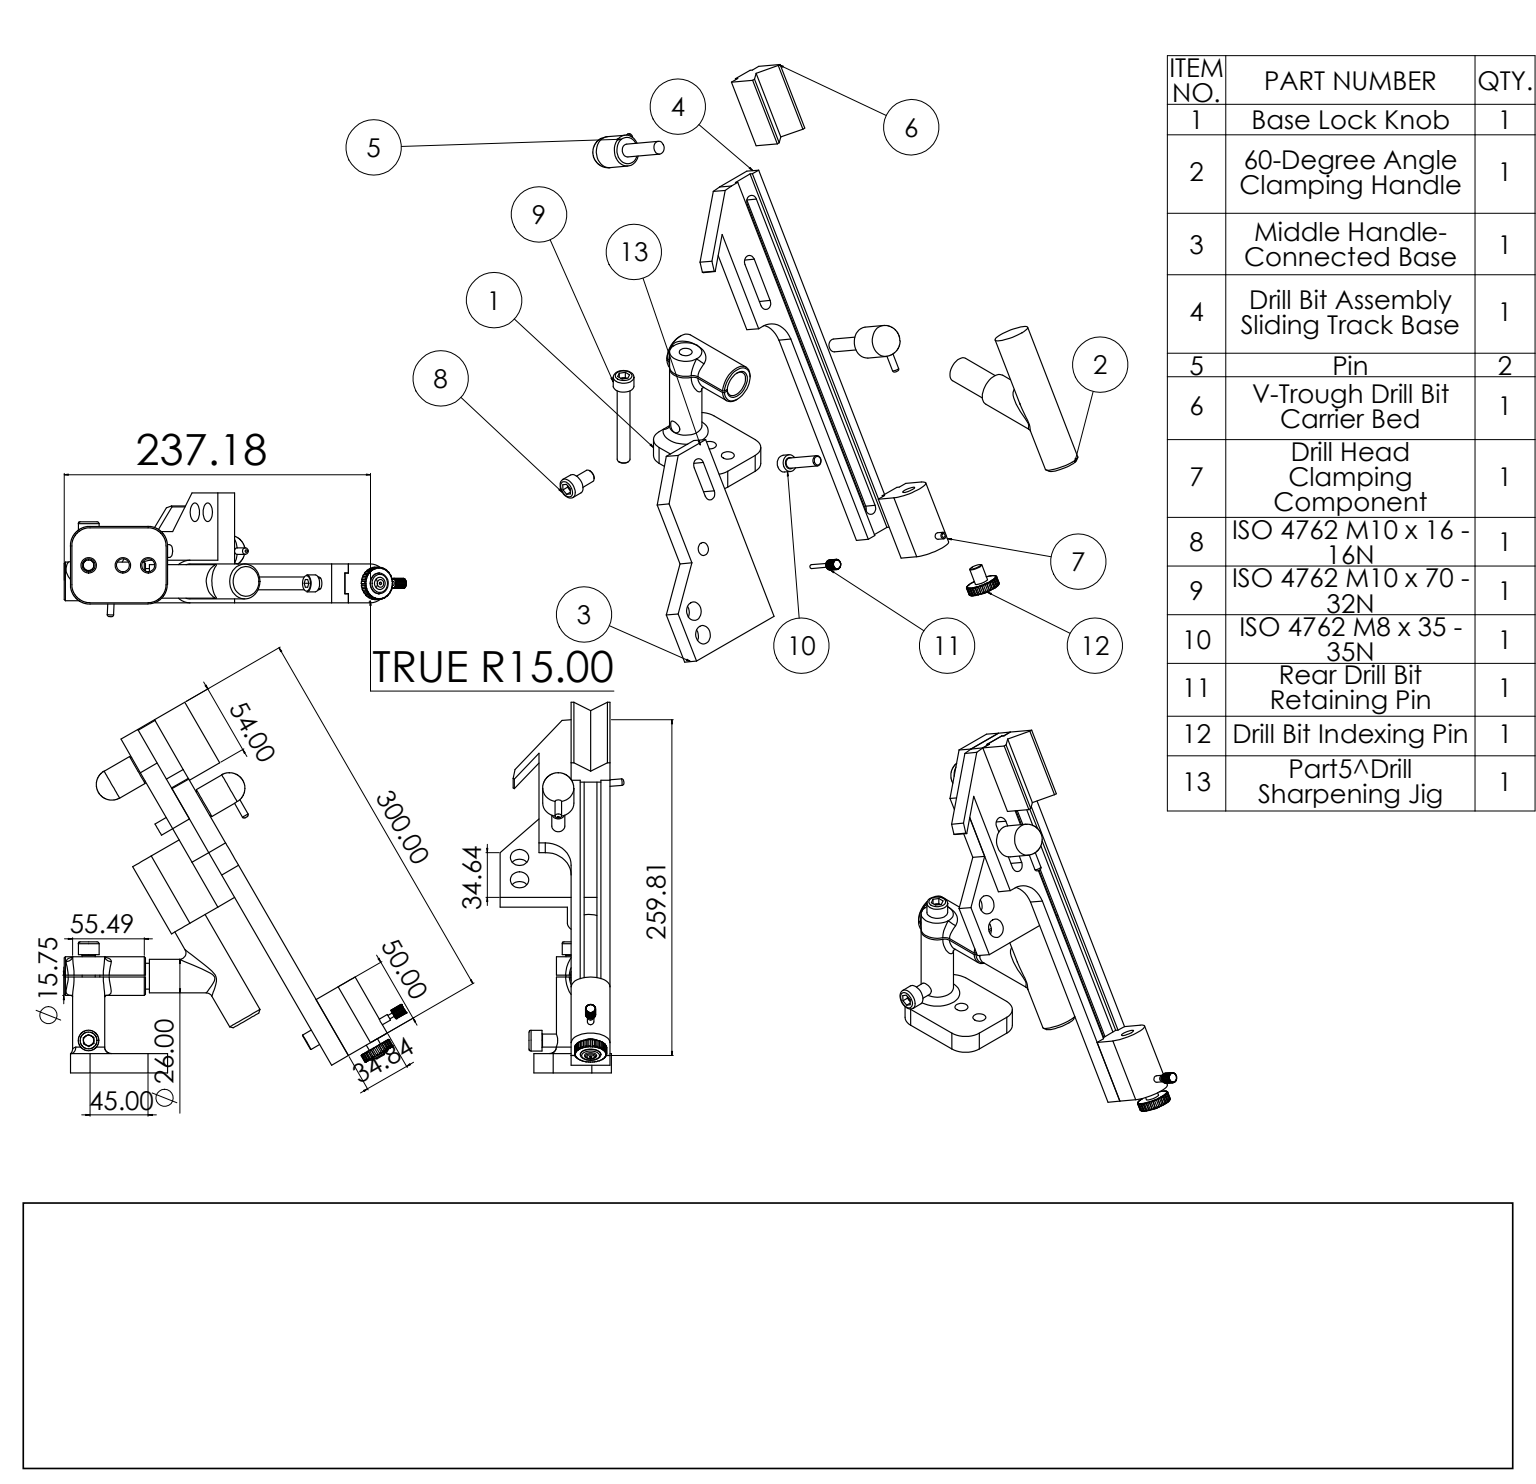
ISO-10303-21;
HEADER;
FILE_DESCRIPTION (('STEP AP214'),
    '1' );
FILE_NAME ('MAS-328',
    '2026-10-26T22:46:44',
    ( '' ),
    ( '' ),
    'SwSTEP 2.0',
    'SolidWorks 2025',
    '' );
FILE_SCHEMA (( 'AUTOMOTIVE_DESIGN' ));
ENDSEC;

DATA;
#1 = PLANE ( 'NONE',  #9182 ) ;
#2 = FACE_OUTER_BOUND ( 'NONE', #11522, .T. ) ;
#3 = CARTESIAN_POINT ( 'NONE',  ( 65.59213978856993776, 73.13321318536134186, -22.65145034150330616 ) ) ;
#4 = DIRECTION ( 'NONE',  ( 0.000000000000000000, 0.4999999999999984457, -0.8660254037844395958 ) ) ;
#5 = DIRECTION ( 'NONE',  ( -0.5000000000000047740, 0.8660254037844358210, 0.000000000000000000 ) ) ;
#6 = ORIENTED_EDGE ( 'NONE', *, *, #8024, .T. ) ;
#7 = CARTESIAN_POINT ( 'NONE',  ( 63.07699891084844523, 77.89006876494195808, -8.475025019650114899 ) ) ;
#8 = VECTOR ( 'NONE', #14091, 1000.000000000000227 ) ;
#9 = ORIENTED_EDGE ( 'NONE', *, *, #6510, .F. ) ;
#10 = ORIENTED_EDGE ( 'NONE', *, *, #14818, .T. ) ;
#11 = CARTESIAN_POINT ( 'NONE',  ( 221.3517569193846271, 32.83641968311255965, -11.78314368930809231 ) ) ;
#12 = CARTESIAN_POINT ( 'NONE',  ( 221.2462657448135417, 31.50562936879607889, -12.30768923015401128 ) ) ;
#13 = EDGE_CURVE ( 'NONE', #4124, #14697, #820, .T. ) ;
#14 = ORIENTED_EDGE ( 'NONE', *, *, #6610, .T. ) ;
#15 = CARTESIAN_POINT ( 'NONE',  ( -25.96080279087190945, 79.85293219504170281, -10.39653350028737755 ) ) ;
#16 = DIRECTION ( 'NONE',  ( -0.8660254037844355990, -0.5000000000000055511, 0.000000000000000000 ) ) ;
#17 = ORIENTED_EDGE ( 'NONE', *, *, #2123, .F. ) ;
#18 = AXIS2_PLACEMENT_3D ( 'NONE', #4792, #10950, #15638 ) ;
#19 = CARTESIAN_POINT ( 'NONE',  ( 0.000000000000000000, -10.00000000000000000, 0.000000000000000000 ) ) ;
#20 = LINE ( 'NONE', #125, #6600 ) ;
#21 = LINE ( 'NONE', #16230, #18993 ) ;
#22 = VECTOR ( 'NONE', #7023, 1000.000000000000114 ) ;
#23 = FACE_OUTER_BOUND ( 'NONE', #2829, .T. ) ;
#24 = CARTESIAN_POINT ( 'NONE',  ( 211.0853526979653907, 12.80985690719961312, -24.65893733905802776 ) ) ;
#25 = AXIS2_PLACEMENT_3D ( 'NONE', #18547, #841, #7289 ) ;
#26 = DIRECTION ( 'NONE',  ( 0.5000000000000044409, -0.8660254037844360431, -4.006172263299080068E-16 ) ) ;
#27 = EDGE_CURVE ( 'NONE', #5527, #10122, #12164, .T. ) ;
#28 = DIRECTION ( 'NONE',  ( -0.000000000000000000, 1.355657144061424088E-15, 1.000000000000000000 ) ) ;
#29 = CARTESIAN_POINT ( 'NONE',  ( 227.9553588074475670, 39.88513931160575510, -14.00000000000005507 ) ) ;
#30 = ORIENTED_EDGE ( 'NONE', *, *, #4834, .F. ) ;
#31 = DIRECTION ( 'NONE',  ( -0.2483788854153071712, -0.1434016163555487389, -0.9579895123154875680 ) ) ;
#32 = VECTOR ( 'NONE', #7463, 1000.000000000000114 ) ;
#33 = CARTESIAN_POINT ( 'NONE',  ( 72.20123527641440830, 74.90140838070377072, -0.9291223156572469000 ) ) ;
#34 = LINE ( 'NONE', #11272, #10471 ) ;
#35 = CARTESIAN_POINT ( 'NONE',  ( 214.5488276859554162, 7.740514238813806180, -25.36561010639692881 ) ) ;
#36 = EDGE_CURVE ( 'NONE', #14580, #7029, #1544, .T. ) ;
#38 = VERTEX_POINT ( 'NONE', #5675 ) ;
#37 = EDGE_LOOP ( 'NONE', ( #2124, #18268, #20120, #14576, #10012 ) ) ;
#39 = EDGE_CURVE ( 'NONE', #7899, #11760, #18628, .T. ) ;
#40 = CARTESIAN_POINT ( 'NONE',  ( -32.23733050826358237, 69.70612202061964524, 1.777571403100950187 ) ) ;
#41 = ORIENTED_EDGE ( 'NONE', *, *, #857, .F. ) ;
#42 = CYLINDRICAL_SURFACE ( 'NONE', #6692, 5.000000000000002665 ) ;
#43 = B_SPLINE_CURVE_WITH_KNOTS ( 'NONE', 3,
 ( #9463, #2715, #6285, #20719 ),
 .UNSPECIFIED., .F., .F.,
 ( 4, 4 ),
 ( 9.419794497943025677E-05, 0.0009481836829574997018 ),
 .UNSPECIFIED. ) ;
#44 = CARTESIAN_POINT ( 'NONE',  ( -28.41953442586123302, 80.00000000005270806, -1.424835221693572684 ) ) ;
#45 = CARTESIAN_POINT ( 'NONE',  ( 43.00000000000000000, 0.000000000000000000, 0.000000000000000000 ) ) ;
#46 = VECTOR ( 'NONE', #10219, 1000.000000000000227 ) ;
#47 = CIRCLE ( 'NONE', #14620, 8.000000000000058620 ) ;
#48 = CARTESIAN_POINT ( 'NONE',  ( 218.4949601902774248, 36.27103037639907512, -10.80501622924627902 ) ) ;
#49 = AXIS2_PLACEMENT_3D ( 'NONE', #5119, #19642, #8405 ) ;
#50 = CARTESIAN_POINT ( 'NONE',  ( 54.22345804136912051, 78.00945976696758066, -12.46744236580036791 ) ) ;
#51 = PRODUCT_RELATED_PRODUCT_CATEGORY ( 'part', '', ( #13821 ) ) ;
#52 = LINE ( 'NONE', #20812, #10386 ) ;
#53 = ORIENTED_EDGE ( 'NONE', *, *, #309, .F. ) ;
#54 =( LENGTH_UNIT ( ) NAMED_UNIT ( * ) SI_UNIT ( .MILLI., .METRE. ) );
#55 = PLANE ( 'NONE',  #11183 ) ;
#56 = ORIENTED_EDGE ( 'NONE', *, *, #8456, .T. ) ;
#57 = CARTESIAN_POINT ( 'NONE',  ( 80.00000000000000000, 0.000000000000000000, 0.000000000000000000 ) ) ;
#58 = ADVANCED_FACE ( 'NONE', ( #8662 ), #15261, .F. ) ;
#59 = AXIS2_PLACEMENT_3D ( 'NONE', #20205, #816, #18936 ) ;
#60 = ORIENTED_EDGE ( 'NONE', *, *, #4152, .T. ) ;
#61 = EDGE_CURVE ( 'NONE', #19064, #20850, #19152, .T. ) ;
#62 = LINE ( 'NONE', #1856, #5490 ) ;
#63 = CARTESIAN_POINT ( 'NONE',  ( 213.9541640218532166, 4.979392293579961937, -14.00000000000005507 ) ) ;
#64 = CARTESIAN_POINT ( 'NONE',  ( 220.2412569556373398, 35.17173234550051575, -17.78601433598970871 ) ) ;
#65 = CIRCLE ( 'NONE', #5111, 12.50000000000000000 ) ;
#66 = B_SPLINE_CURVE_WITH_KNOTS ( 'NONE', 3,
 ( #8841, #10417, #10308, #18497, #16902, #3750, #6925, #16700, #20081, #8735, #685, #15341, #16481, #1963, #8630, #5225, #15026, #3643, #15129, #584, #2382, #3544, #11613, #795, #7034, #9988, #7140, #8411, #10096, #5431, #7246, #2073, #5545, #13520, #19652, #19965, #12034, #14912, #20596, #12135, #15751, #14164, #15438, #7666 ),
 .UNSPECIFIED., .F., .F.,
 ( 4, 2, 2, 2, 2, 2, 2, 2, 2, 2, 2, 2, 2, 2, 2, 2, 2, 2, 2, 2, 2, 4 ),
 ( 0.09617483233575800650, 0.09914136407045009980, 0.1006246299377961534, 0.1021078958051422070, 0.1050744275398343142, 0.1080409592745264352, 0.1095242251418725027, 0.1110074910092185702, 0.1139740227439106635, 0.1154572886112567032, 0.1169405544786027568, 0.1176821874122757766, 0.1184238203459488104, 0.1199070862132948084, 0.1213903520806408065, 0.1228736179479868185, 0.1258401496826788146, 0.1288066814173708385, 0.1317732131520628625, 0.1377062766214468548, 0.1406728083561389064, 0.1436393400908309581 ),
 .UNSPECIFIED. ) ;
#67 = AXIS2_PLACEMENT_3D ( 'NONE', #10593, #11884, #4139 ) ;
#68 = CARTESIAN_POINT ( 'NONE',  ( 204.1847125716027733, 2.529609678273321727, -2.551678190571418092 ) ) ;
#69 = CARTESIAN_POINT ( 'NONE',  ( -27.55705705607979894, 6.378909713838078588, -4.810857297669037358 ) ) ;
#70 = CARTESIAN_POINT ( 'NONE',  ( 192.7136026671465174, 6.680946580180795458, -11.01983352639493141 ) ) ;
#71 = ORIENTED_EDGE ( 'NONE', *, *, #7515, .F. ) ;
#72 = ADVANCED_FACE ( 'NONE', ( #4104, #6856 ), #20110, .T. ) ;
#73 = DIRECTION ( 'NONE',  ( -1.000000000000000000, -0.000000000000000000, -0.000000000000000000 ) ) ;
#74 = CARTESIAN_POINT ( 'NONE',  ( -3.712242387446013758, 47.26449505096422854, -2.316332963494041497 ) ) ;
#75 = AXIS2_PLACEMENT_3D ( 'NONE', #8179, #20707, #4902 ) ;
#76 = ORIENTED_EDGE ( 'NONE', *, *, #3037, .F. ) ;
#77 = CARTESIAN_POINT ( 'NONE',  ( 199.2231352798573027, 21.03391272677540513, -14.00000000000005507 ) ) ;
#78 = CARTESIAN_POINT ( 'NONE',  ( -4.898149591010308335, 50.01850704181430984, -13.27720951148779349 ) ) ;
#79 = CARTESIAN_POINT ( 'NONE',  ( 25.17200000000003612, 0.000000000000000000, 0.000000000000000000 ) ) ;
#80 = VECTOR ( 'NONE', #13900, 1000.000000000000227 ) ;
#81 = AXIS2_PLACEMENT_3D ( 'NONE', #9573, #7982, #13089 ) ;
#82 = EDGE_CURVE ( 'NONE', #14650, #1521, #9980, .T. ) ;
#83 = CARTESIAN_POINT ( 'NONE',  ( 215.3534639294407782, 15.62807865697965504, -9.913166705713923221 ) ) ;
#84 = AXIS2_PLACEMENT_3D ( 'NONE', #10451, #8972, #10240 ) ;
#85 = CARTESIAN_POINT ( 'NONE',  ( 218.1772659767879361, 38.33479928385730062, -13.56204498775452372 ) ) ;
#87 = ORIENTED_EDGE ( 'NONE', *, *, #4132, .T. ) ;
#86 = ORIENTED_EDGE ( 'NONE', *, *, #18700, .F. ) ;
#88 = EDGE_LOOP ( 'NONE', ( #5156, #19517 ) ) ;
#89 = CARTESIAN_POINT ( 'NONE',  ( 204.5373383384513772, 2.217977392850209561, -25.12838443884007944 ) ) ;
#90 = FACE_OUTER_BOUND ( 'NONE', #11303, .T. ) ;
#91 = EDGE_CURVE ( 'NONE', #17637, #19670, #15056, .T. ) ;
#92 = ORIENTED_EDGE ( 'NONE', *, *, #17549, .F. ) ;
#93 = ORIENTED_EDGE ( 'NONE', *, *, #14481, .F. ) ;
#94 = CARTESIAN_POINT ( 'NONE',  ( -20.20766917169448007, 62.83385617594171180, -2.712160011935111914 ) ) ;
#95 = DIRECTION ( 'NONE',  ( -0.5000000000000042188, 0.8660254037844362651, -2.168404344971015524E-16 ) ) ;
#96 = DIRECTION ( 'NONE',  ( 0.7500000000000014433, 0.4330127018922259596, 0.4999999999999919509 ) ) ;
#97 = CARTESIAN_POINT ( 'NONE',  ( -14.59739189792666281, 58.60404727593866170, -4.812026853405405369 ) ) ;
#98 = EDGE_LOOP ( 'NONE', ( #990, #8694, #13068, #17263 ) ) ;
#99 = ORIENTED_EDGE ( 'NONE', *, *, #8969, .F. ) ;
#100 = FACE_OUTER_BOUND ( 'NONE', #9004, .T. ) ;
#101 = AXIS2_PLACEMENT_3D ( 'NONE', #17519, #19410, #6254 ) ;
#102 = ADVANCED_FACE ( 'NONE', ( #18525 ), #10234, .F. ) ;
#103 = CIRCLE ( 'NONE', #7142, 11.94520687646042667 ) ;
#104 = EDGE_CURVE ( 'NONE', #402, #10896, #9651, .T. ) ;
#105 = CARTESIAN_POINT ( 'NONE',  ( 218.1841183754832230, 38.29290577510303706, -13.37096421021187354 ) ) ;
#106 = CARTESIAN_POINT ( 'NONE',  ( 199.3420759002524960, 10.50789738563077513, -26.10173121575770239 ) ) ;
#107 = CARTESIAN_POINT ( 'NONE',  ( -32.72405129661866141, 57.94895811088655080, 0.7443064298479508123 ) ) ;
#108 = CARTESIAN_POINT ( 'NONE',  ( 209.9458835816058411, 16.63000860489531263, -23.47937149798938350 ) ) ;
#109 = ADVANCED_FACE ( 'NONE', ( #2310 ), #10446, .F. ) ;
#110 = FACE_OUTER_BOUND ( 'NONE', #8894, .T. ) ;
#111 = LINE ( 'NONE', #3275, #10000 ) ;
#112 = VERTEX_POINT ( 'NONE', #8556 ) ;
#113 = ORIENTED_EDGE ( 'NONE', *, *, #4613, .F. ) ;
#114 = CARTESIAN_POINT ( 'NONE',  ( 60.67510459333478678, 75.25732190833497270, -4.504626686252581891 ) ) ;
#115 = ORIENTED_EDGE ( 'NONE', *, *, #18818, .F. ) ;
#116 = DIRECTION ( 'NONE',  ( -0.8660254037844363761, -0.5000000000000043299, 6.872020471724002955E-17 ) ) ;
#117 = DIRECTION ( 'NONE',  ( -0.5000000000000029976, 0.8660254037844370423, 0.000000000000000000 ) ) ;
#118 = EDGE_CURVE ( 'NONE', #7633, #8779, #11849, .T. ) ;
#119 = ORIENTED_EDGE ( 'NONE', *, *, #8707, .T. ) ;
#120 = CARTESIAN_POINT ( 'NONE',  ( 184.9952905943350743, 3.535126980567765642, 0.9999999999999187317 ) ) ;
#121 = DIRECTION ( 'NONE',  ( -0.7071067811865331398, 8.659560562355110352E-17, -0.7071067811865620056 ) ) ;
#122 = VERTEX_POINT ( 'NONE', #2105 ) ;
#123 = APPLICATION_CONTEXT ( 'automotive_design' ) ;
#124 = CYLINDRICAL_SURFACE ( 'NONE', #4697, 7.155882939242642848 ) ;
#125 = CARTESIAN_POINT ( 'NONE',  ( 74.11964624731606932, 223.5773763115391262, -13.99999999999998757 ) ) ;
#126 = CARTESIAN_POINT ( 'NONE',  ( -0.1767699604045824824, 64.25000000000000000, 2.481238266578627449 ) ) ;
#127 = CARTESIAN_POINT ( 'NONE',  ( 221.7203120311961584, 32.40398170487073770, -15.50530648567724157 ) ) ;
#128 = DIRECTION ( 'NONE',  ( 0.5000000000000054401, -0.8660254037844354880, 0.000000000000000000 ) ) ;
#129 = DIRECTION ( 'NONE',  ( 0.000000000000000000, -0.5000000000000009992, -0.8660254037844380415 ) ) ;
#130 = CARTESIAN_POINT ( 'NONE',  ( 43.00000000000000000, 4.052968581778165278E-16, -3.309499999999999886 ) ) ;
#131 = ORIENTED_EDGE ( 'NONE', *, *, #17184, .F. ) ;
#132 = ORIENTED_EDGE ( 'NONE', *, *, #6398, .F. ) ;
#133 = DIRECTION ( 'NONE',  ( -0.000000000000000000, 1.000000000000000000, -0.000000000000000000 ) ) ;
#134 = CARTESIAN_POINT ( 'NONE',  ( 79.71489363099678371, 68.48589378271981332, 0.4850882486192328313 ) ) ;
#135 = CARTESIAN_POINT ( 'NONE',  ( 221.3208164193364951, 32.89001020120745267, -16.29291827778590118 ) ) ;
#136 = AXIS2_PLACEMENT_3D ( 'NONE', #13684, #12192, #17075 ) ;
#137 = CARTESIAN_POINT ( 'NONE',  ( 78.24291704612552678, 52.61578353862905288, -16.49051273642769289 ) ) ;
#138 = VECTOR ( 'NONE', #4761, 1000.000000000000114 ) ;
#140 = VERTEX_POINT ( 'NONE', #15368 ) ;
#139 = VERTEX_POINT ( 'NONE', #19892 ) ;
#141 = CARTESIAN_POINT ( 'NONE',  ( 226.3069872472380837, 42.74020260364054025, -12.62147488791602612 ) ) ;
#142 = VERTEX_POINT ( 'NONE', #18313 ) ;
#143 = CARTESIAN_POINT ( 'NONE',  ( -31.87136685185827645, 66.76123571212177410, 2.404802591979305237 ) ) ;
#144 = ORIENTED_EDGE ( 'NONE', *, *, #2804, .F. ) ;
#145 = CYLINDRICAL_SURFACE ( 'NONE', #15851, 12.47473710546057646 ) ;
#146 = DIRECTION ( 'NONE',  ( -1.000000000000000000, -0.000000000000000000, -0.000000000000000000 ) ) ;
#147 = CARTESIAN_POINT ( 'NONE',  ( 59.39721438298058587, 215.0773763115390125, -5.999999999999973355 ) ) ;
#148 = AXIS2_PLACEMENT_3D ( 'NONE', #15807, #6608, #5027 ) ;
#149 = CARTESIAN_POINT ( 'NONE',  ( 55.21771490548105987, 77.58705400462579860, -9.223793769219156502 ) ) ;
#150 = EDGE_CURVE ( 'NONE', #14752, #17095, #8765, .T. ) ;
#151 = CARTESIAN_POINT ( 'NONE',  ( -28.39898833977742854, 64.25000000000000000, 3.829121630900767848 ) ) ;
#152 = ORIENTED_EDGE ( 'NONE', *, *, #1114, .F. ) ;
#153 = DIRECTION ( 'NONE',  ( 0.8660254037844380415, 0.5000000000000014433, 0.000000000000000000 ) ) ;
#154 = CARTESIAN_POINT ( 'NONE',  ( 189.6713070174558311, 31.72030020615783030, -9.000000000000065725 ) ) ;
#155 = ORIENTED_EDGE ( 'NONE', *, *, #17412, .T. ) ;
#156 = CARTESIAN_POINT ( 'NONE',  ( 220.9239438240024356, 32.06390731203414646, -15.46846178913028425 ) ) ;
#157 = EDGE_LOOP ( 'NONE', ( #6682, #1571, #19730, #8704 ) ) ;
#158 = CARTESIAN_POINT ( 'NONE',  ( 217.8938201104045618, 37.31223553720490571, -11.78314368930801770 ) ) ;
#159 = DIRECTION ( 'NONE',  ( 0.5000000000000054401, -0.8660254037844353769, 3.330669073875469128E-16 ) ) ;
#160 = LINE ( 'NONE', #8201, #12763 ) ;
#161 = AXIS2_PLACEMENT_3D ( 'NONE', #9354, #1324, #10848 ) ;
#162 = EDGE_CURVE ( 'NONE', #4703, #13744, #13389, .T. ) ;
#163 = CARTESIAN_POINT ( 'NONE',  ( 204.3649803021097568, 2.376073449241438595, -2.709673684914560621 ) ) ;
#164 = CARTESIAN_POINT ( 'NONE',  ( 228.9348979434486466, 38.18852776005019223, -17.77545290933962008 ) ) ;
#165 = CARTESIAN_POINT ( 'NONE',  ( 226.5371121300225923, 42.34161461457158993, -11.75146085096529269 ) ) ;
#166 = VERTEX_POINT ( 'NONE', #7371 ) ;
#167 = CARTESIAN_POINT ( 'NONE',  ( 64.57205371728791476, 77.00255147951500589, -18.47244162738281048 ) ) ;
#168 = CARTESIAN_POINT ( 'NONE',  ( -15.61408887313298166, 45.63508326896292289, -12.50000000000000533 ) ) ;
#169 = EDGE_CURVE ( 'NONE', #12266, #578, #4413, .T. ) ;
#170 = ORIENTED_EDGE ( 'NONE', *, *, #16678, .F. ) ;
#171 = EDGE_CURVE ( 'NONE', #6173, #11821, #2564, .T. ) ;
#172 = LINE ( 'NONE', #6717, #1739 ) ;
#173 = CARTESIAN_POINT ( 'NONE',  ( 0.8637328751229490509, 57.32143202600091314, 0.4056442452730588677 ) ) ;
#174 = CARTESIAN_POINT ( 'NONE',  ( 0.2936549083987780584, 78.35468191082874512, -5.667085693055155637 ) ) ;
#175 = DIRECTION ( 'NONE',  ( 0.8660254037844373753, 0.5000000000000021094, -5.551115123125781716E-16 ) ) ;
#176 = DIRECTION ( 'NONE',  ( 1.000000000000000000, 0.000000000000000000, 0.000000000000000000 ) ) ;
#177 = VECTOR ( 'NONE', #19876, 1000.000000000000114 ) ;
#179 = EDGE_LOOP ( 'NONE', ( #14684, #11009, #8415, #3507 ) ) ;
#178 = ORIENTED_EDGE ( 'NONE', *, *, #4682, .F. ) ;
#180 = ORIENTED_EDGE ( 'NONE', *, *, #8626, .T. ) ;
#181 = EDGE_LOOP ( 'NONE', ( #14178, #14869, #3890, #5041 ) ) ;
#182 = CARTESIAN_POINT ( 'NONE',  ( 5.000000000000004441, -2.342598717236899830, 4.057500000000059615 ) ) ;
#183 = DIRECTION ( 'NONE',  ( 0.000000000000000000, 0.000000000000000000, -1.000000000000000000 ) ) ;
#184 = VERTEX_POINT ( 'NONE', #12380 ) ;
#185 = ORIENTED_EDGE ( 'NONE', *, *, #2629, .T. ) ;
#186 = EDGE_CURVE ( 'NONE', #5696, #10545, #15103, .T. ) ;
#187 = CARTESIAN_POINT ( 'NONE',  ( 31.00000000000000711, 65.00000000000000000, 0.4999999999999970024 ) ) ;
#188 = CARTESIAN_POINT ( 'NONE',  ( 61.55523633728010680, 134.3395726428436774, -12.50000000000000000 ) ) ;
#189 = DIRECTION ( 'NONE',  ( -0.8660254037844360431, -0.5000000000000044409, 5.976026924694052093E-17 ) ) ;
#190 = CARTESIAN_POINT ( 'NONE',  ( 5.000000000000000000, -4.685197434473809430, 6.071532165918824830E-15 ) ) ;
#191 = ORIENTED_EDGE ( 'NONE', *, *, #11432, .T. ) ;
#192 = ORIENTED_EDGE ( 'NONE', *, *, #8358, .F. ) ;
#193 = CARTESIAN_POINT ( 'NONE',  ( 227.1212915979693037, 40.35032020428622701, -17.81526153211078523 ) ) ;
#194 = VECTOR ( 'NONE', #13444, 1000.000000000000000 ) ;
#195 = EDGE_CURVE ( 'NONE', #20338, #18465, #2729, .T. ) ;
#196 = VECTOR ( 'NONE', #4579, 1000.000000000000000 ) ;
#197 = VECTOR ( 'NONE', #8588, 1000.000000000000227 ) ;
#198 = PLANE ( 'NONE',  #5711 ) ;
#199 = ADVANCED_FACE ( 'NONE', ( #15570 ), #12386, .T. ) ;
#200 = CARTESIAN_POINT ( 'NONE',  ( 228.4406543832519674, 38.06511682656112328, -17.45257705044836172 ) ) ;
#201 = CARTESIAN_POINT ( 'NONE',  ( -32.31535884961043337, 59.90787884595005863, 1.627344972937480483 ) ) ;
#202 = CARTESIAN_POINT ( 'NONE',  ( 206.2111997916997552, 10.34978999605213978, -2.036337243043280676 ) ) ;
#203 = ORIENTED_EDGE ( 'NONE', *, *, #13292, .F. ) ;
#204 = DIRECTION ( 'NONE',  ( 0.8660254037844361541, 0.5000000000000043299, -5.976026924694053325E-17 ) ) ;
#205 = CARTESIAN_POINT ( 'NONE',  ( 221.1274251996601663, 33.84282198876892522, -17.45257705044835816 ) ) ;
#206 = VERTEX_POINT ( 'NONE', #13865 ) ;
#207 = CARTESIAN_POINT ( 'NONE',  ( 54.88115708448756891, 77.73008567377026168, -9.852707893755395574 ) ) ;
#208 = EDGE_CURVE ( 'NONE', #2385, #6975, #20515, .T. ) ;
#209 = ORIENTED_EDGE ( 'NONE', *, *, #20399, .T. ) ;
#210 = EDGE_CURVE ( 'NONE', #4589, #15417, #7306, .T. ) ;
#211 = VECTOR ( 'NONE', #12529, 1000.000000000000114 ) ;
#212 = CARTESIAN_POINT ( 'NONE',  ( 206.9147384664715048, 10.75597823931694563, -16.91825718831810477 ) ) ;
#213 = CIRCLE ( 'NONE', #14445, 0.4000000000000001887 ) ;
#214 = ORIENTED_EDGE ( 'NONE', *, *, #1106, .F. ) ;
#215 = CARTESIAN_POINT ( 'NONE',  ( 220.3379489458267528, 34.59238660243320851, -17.48830818005197330 ) ) ;
#216 = ORIENTED_EDGE ( 'NONE', *, *, #15468, .T. ) ;
#217 = ITEM_DEFINED_TRANSFORMATION ( 'NONE', 'NONE', #8397,  #18233 ) ;
#218 = EDGE_CURVE ( 'NONE', #14678, #19163, #6091, .T. ) ;
#219 = CARTESIAN_POINT ( 'NONE',  ( 203.2433706042751282, 14.07066088650062241, -14.00000000000004974 ) ) ;
#220 = ORIENTED_EDGE ( 'NONE', *, *, #3519, .T. ) ;
#221 = CIRCLE ( 'NONE', #10696, 3.047499999999999876 ) ;
#222 = FACE_OUTER_BOUND ( 'NONE', #14547, .T. ) ;
#223 = CYLINDRICAL_SURFACE ( 'NONE', #8286, 5.000000000000000000 ) ;
#224 = CIRCLE ( 'NONE', #4614, 1.000000000000000888 ) ;
#225 = CARTESIAN_POINT ( 'NONE',  ( 58.57586221349340860, 85.49999999999941735, -12.75852093573072032 ) ) ;
#226 = CARTESIAN_POINT ( 'NONE',  ( 9.999999999999994671, 5.551115123125782702E-17, 8.000000000000058620 ) ) ;
#227 = ADVANCED_FACE ( 'NONE', ( #9070 ), #12693, .F. ) ;
#228 = EDGE_LOOP ( 'NONE', ( #1966, #14551, #9394, #914, #2067, #12471, #14821, #17580, #5403, #1919 ) ) ;
#229 = DIRECTION ( 'NONE',  ( -0.5000000000000046629, 0.8660254037844360431, -0.000000000000000000 ) ) ;
#230 = DIRECTION ( 'NONE',  ( -0.5000000000000049960, 0.8660254037844358210, -0.000000000000000000 ) ) ;
#231 = DIRECTION ( 'NONE',  ( 0.8660254037844360431, 0.5000000000000044409, -5.976026924694052093E-17 ) ) ;
#232 = ORIENTED_EDGE ( 'NONE', *, *, #19491, .T. ) ;
#233 = DIRECTION ( 'NONE',  ( -0.8660254037844354880, -0.5000000000000055511, 0.000000000000000000 ) ) ;
#234 = ADVANCED_FACE ( 'NONE', ( #2627 ), #13079, .T. ) ;
#235 = CARTESIAN_POINT ( 'NONE',  ( 82.91273300024698756, 62.96352848655696732, 0.4857625843512909936 ) ) ;
#236 = CARTESIAN_POINT ( 'NONE',  ( 221.3640885658708441, 32.78503583879686545, -16.13347615800341472 ) ) ;
#237 = CARTESIAN_POINT ( 'NONE',  ( 79.37077236198800279, 49.52807498578272316, -11.55216451523023657 ) ) ;
#239 = ORIENTED_EDGE ( 'NONE', *, *, #5233, .T. ) ;
#238 = EDGE_LOOP ( 'NONE', ( #4211, #12688, #8856, #3660 ) ) ;
#240 = ORIENTED_EDGE ( 'NONE', *, *, #10844, .T. ) ;
#241 = AXIS2_PLACEMENT_3D ( 'NONE', #8090, #7996, #6604 ) ;
#242 = ORIENTED_EDGE ( 'NONE', *, *, #18363, .T. ) ;
#243 = UNCERTAINTY_MEASURE_WITH_UNIT (LENGTH_MEASURE( 1.000000000000000082E-05 ), #16702, 'distance_accuracy_value', 'NONE');
#244 = DIRECTION ( 'NONE',  ( -0.5000000000000049960, 0.8660254037844357100, -0.000000000000000000 ) ) ;
#245 = VERTEX_POINT ( 'NONE', #13977 ) ;
#246 = DIRECTION ( 'NONE',  ( 1.000000000000000000, 0.000000000000000000, 0.000000000000000000 ) ) ;
#247 = FACE_OUTER_BOUND ( 'NONE', #3115, .T. ) ;
#248 = CARTESIAN_POINT ( 'NONE',  ( 215.3457899893760725, 15.62364810561754958, -18.11117897393244647 ) ) ;
#249 = CARTESIAN_POINT ( 'NONE',  ( 217.4786251556303682, 38.03137429392004520, -11.78784277354600540 ) ) ;
#250 = CARTESIAN_POINT ( 'NONE',  ( 69.27805541368826425, 71.51676853726520733, -1.217222206000668994 ) ) ;
#251 = LINE ( 'NONE', #16684, #18558 ) ;
#252 = ORIENTED_EDGE ( 'NONE', *, *, #4604, .T. ) ;
#254 = FACE_OUTER_BOUND ( 'NONE', #19401, .T. ) ;
#253 = AXIS2_PLACEMENT_3D ( 'NONE', #1126, #2508, #8850 ) ;
#255 = VERTEX_POINT ( 'NONE', #1143 ) ;
#256 = DIRECTION ( 'NONE',  ( 1.000000000000000000, 0.000000000000000000, 0.000000000000000000 ) ) ;
#257 = ORIENTED_EDGE ( 'NONE', *, *, #4813, .T. ) ;
#258 = CARTESIAN_POINT ( 'NONE',  ( 204.4631859798315361, 9.340573751222835952, -1.438440158918556255 ) ) ;
#259 = FACE_OUTER_BOUND ( 'NONE', #238, .T. ) ;
#260 = CARTESIAN_POINT ( 'NONE',  ( 216.5552780741873278, 15.79089711517258188, -12.53629070788368338 ) ) ;
#261 = CARTESIAN_POINT ( 'NONE',  ( 4.000000000000000000, 1.759474945355379960, -3.047500000000001652 ) ) ;
#262 = VECTOR ( 'NONE', #1217, 1000.000000000000000 ) ;
#263 = EDGE_CURVE ( 'NONE', #15664, #11736, #7688, .T. ) ;
#264 = CARTESIAN_POINT ( 'NONE',  ( 219.4389998921951133, 34.63590564831543617, -18.24372585368656630 ) ) ;
#265 = CARTESIAN_POINT ( 'NONE',  ( 227.4113091407688785, 39.84799508507109067, -17.89498551959672312 ) ) ;
#266 = ORIENTED_EDGE ( 'NONE', *, *, #16288, .F. ) ;
#267 = VECTOR ( 'NONE', #19215, 1000.000000000000227 ) ;
#268 = CARTESIAN_POINT ( 'NONE',  ( 79.94330251453826008, 67.07585766759784462, -25.35419664930641659 ) ) ;
#269 = CARTESIAN_POINT ( 'NONE',  ( -4.599716269004222369, 61.16723911170964811, 5.137000474222295665 ) ) ;
#270 = VERTEX_POINT ( 'NONE', #17044 ) ;
#271 = B_SPLINE_CURVE_WITH_KNOTS ( 'NONE', 3,
 ( #15574, #20319, #4421, #12593 ),
 .UNSPECIFIED., .F., .F.,
 ( 4, 4 ),
 ( 3.854193985297353114E-07, 0.0008543711573825201388 ),
 .UNSPECIFIED. ) ;
#272 = CARTESIAN_POINT ( 'NONE',  ( 227.4113091407688785, 39.84799508507109067, -17.89498551959672312 ) ) ;
#273 = CARTESIAN_POINT ( 'NONE',  ( 1.235636163673195176, 55.55531401624686794, -0.8411524222362073422 ) ) ;
#274 = CARTESIAN_POINT ( 'NONE',  ( -27.29860958162435480, 65.74999999999997158, 5.347094680480812379 ) ) ;
#275 = LINE ( 'NONE', #15144, #3748 ) ;
#276 = DIRECTION ( 'NONE',  ( 0.000000000000000000, 0.000000000000000000, -1.000000000000000000 ) ) ;
#277 = EDGE_CURVE ( 'NONE', #4589, #9756, #12406, .T. ) ;
#278 = CARTESIAN_POINT ( 'NONE',  ( -28.99999999999999289, 0.000000000000000000, 15.00000000000000178 ) ) ;
#280 = EDGE_LOOP ( 'NONE', ( #9635, #17921, #8883, #13281 ) ) ;
#279 = VERTEX_POINT ( 'NONE', #5885 ) ;
#281 = ORIENTED_EDGE ( 'NONE', *, *, #10002, .F. ) ;
#282 = ORIENTED_EDGE ( 'NONE', *, *, #5023, .T. ) ;
#283 = DIRECTION ( 'NONE',  ( -0.8660254037844370423, -0.5000000000000027756, 0.000000000000000000 ) ) ;
#284 = B_SPLINE_CURVE_WITH_KNOTS ( 'NONE', 3,
 ( #15872, #6200, #7896, #7588 ),
 .UNSPECIFIED., .F., .F.,
 ( 4, 4 ),
 ( 5.392423665328082974E-07, 0.0008545249803445767369 ),
 .UNSPECIFIED. ) ;
#285 = FACE_OUTER_BOUND ( 'NONE', #6570, .T. ) ;
#286 = ORIENTED_EDGE ( 'NONE', *, *, #8772, .T. ) ;
#287 = EDGE_LOOP ( 'NONE', ( #14816, #1290 ) ) ;
#288 = CARTESIAN_POINT ( 'NONE',  ( 229.5015552748991752, 36.55408933899362012, -12.94088743653098383 ) ) ;
#289 = DIRECTION ( 'NONE',  ( 0.000000000000000000, -6.938893903907176763E-18, -1.000000000000000000 ) ) ;
#290 = DIRECTION ( 'NONE',  ( -0.4999999999999995004, 0.8660254037844390407, 0.000000000000000000 ) ) ;
#291 = CARTESIAN_POINT ( 'NONE',  ( 213.7304257015346423, 14.51400719500950132, -6.188753603160008332 ) ) ;
#292 = ORIENTED_EDGE ( 'NONE', *, *, #18582, .T. ) ;
#293 = ADVANCED_FACE ( 'NONE', ( #8966 ), #1343, .F. ) ;
#294 = ORIENTED_EDGE ( 'NONE', *, *, #17027, .F. ) ;
#295 = EDGE_CURVE ( 'NONE', #10545, #10364, #20522, .T. ) ;
#296 = DIRECTION ( 'NONE',  ( 0.5943026915289653100, 0.3431208189343725179, 0.7273736415730454041 ) ) ;
#297 = AXIS2_PLACEMENT_3D ( 'NONE', #15625, #6046, #20370 ) ;
#298 = CARTESIAN_POINT ( 'NONE',  ( 191.0833833835251880, 36.99024094849657018, -18.91295074164679235 ) ) ;
#299 =( BOUNDED_CURVE ( )  B_SPLINE_CURVE ( 3, ( #3480, #412, #16318, #298 ),
 .UNSPECIFIED., .F., .F. ) 
 B_SPLINE_CURVE_WITH_KNOTS ( ( 4, 4 ),
 ( 1.570796326794896114, 1.757668500643543075 ),
 .UNSPECIFIED. ) 
 CURVE ( )  GEOMETRIC_REPRESENTATION_ITEM ( )  RATIONAL_B_SPLINE_CURVE ( ( 1.000000000000000000, 0.9970920157757051649, 0.9970920157757051649, 1.000000000000000000 ) ) 
 REPRESENTATION_ITEM ( '' )  );
#300 = LINE ( 'NONE', #11651, #4810 ) ;
#301 = CARTESIAN_POINT ( 'NONE',  ( -33.51155206502836137, 53.04833639938227208, -3.407080289749979229 ) ) ;
#302 = CARTESIAN_POINT ( 'NONE',  ( 5.000000000000000000, 4.685197434473812983, -6.938893903907228378E-15 ) ) ;
#303 = CARTESIAN_POINT ( 'NONE',  ( 205.0644204223817439, 9.510686714291797017, -26.12768996730766347 ) ) ;
#304 = CARTESIAN_POINT ( 'NONE',  ( 227.5312376355471145, 39.64027283883993391, -14.00000000000005507 ) ) ;
#305 = VERTEX_POINT ( 'NONE', #18938 ) ;
#306 = ORIENTED_EDGE ( 'NONE', *, *, #3575, .F. ) ;
#307 = EDGE_CURVE ( 'NONE', #6314, #7288, #8664, .T. ) ;
#309 = EDGE_CURVE ( 'NONE', #20070, #6727, #13759, .T. ) ;
#308 = CARTESIAN_POINT ( 'NONE',  ( 57.74218117268578965, 76.51201622986452833, -6.446212979376384489 ) ) ;
#310 = VERTEX_POINT ( 'NONE', #12278 ) ;
#311 = VECTOR ( 'NONE', #13157, 1000.000000000000000 ) ;
#312 = ORIENTED_EDGE ( 'NONE', *, *, #4694, .F. ) ;
#313 = DIRECTION ( 'NONE',  ( -1.000000000000000000, 0.000000000000000000, 0.000000000000000000 ) ) ;
#314 = DIRECTION ( 'NONE',  ( 0.5000000000000051070, -0.8660254037844358210, 0.000000000000000000 ) ) ;
#315 = EDGE_CURVE ( 'NONE', #14969, #8807, #10929, .T. ) ;
#316 = ORIENTED_EDGE ( 'NONE', *, *, #15267, .F. ) ;
#317 = CARTESIAN_POINT ( 'NONE',  ( 207.3576251285122112, 11.01167897286662800, -2.341985411377013548 ) ) ;
#318 = CONTEXT_DEPENDENT_SHAPE_REPRESENTATION ( #20570, #7202 ) ;
#319 = EDGE_CURVE ( 'NONE', #17948, #11709, #17482, .T. ) ;
#320 = DIRECTION ( 'NONE',  ( -0.8660254037844355990, -0.5000000000000055511, 0.000000000000000000 ) ) ;
#321 = ORIENTED_EDGE ( 'NONE', *, *, #9028, .T. ) ;
#322 = DIRECTION ( 'NONE',  ( 0.4586056507527268011, -0.7943282877419131083, -0.3984010898462360672 ) ) ;
#323 = CARTESIAN_POINT ( 'NONE',  ( 209.1177676012032407, 5.377710327540435209, -26.45271578590685380 ) ) ;
#324 = EDGE_CURVE ( 'NONE', #1328, #16503, #11374, .T. ) ;
#325 = AXIS2_PLACEMENT_3D ( 'NONE', #1147, #20520, #11965 ) ;
#326 = ORIENTED_EDGE ( 'NONE', *, *, #16117, .T. ) ;
#327 = DIRECTION ( 'NONE',  ( -0.5000000000000025535, 0.8660254037844372643, 0.000000000000000000 ) ) ;
#328 = DIRECTION ( 'NONE',  ( 0.9537419254229496657, 0.000000000000000000, 0.3006265784832155008 ) ) ;
#329 = AXIS2_PLACEMENT_3D ( 'NONE', #7780, #14388, #14489 ) ;
#330 = VERTEX_POINT ( 'NONE', #3444 ) ;
#331 = CARTESIAN_POINT ( 'NONE',  ( 0.000000000000000000, 3.518949890710767026, -4.987329993433320396E-15 ) ) ;
#332 = VECTOR ( 'NONE', #6843, 1000.000000000000114 ) ;
#333 = DIRECTION ( 'NONE',  ( 0.000000000000000000, 0.8660254037844380415, -0.5000000000000009992 ) ) ;
#334 = FACE_OUTER_BOUND ( 'NONE', #6241, .T. ) ;
#335 = ORIENTED_EDGE ( 'NONE', *, *, #7992, .F. ) ;
#337 = EDGE_CURVE ( 'NONE', #14688, #14554, #8312, .T. ) ;
#336 = PLANE ( 'NONE',  #16281 ) ;
#338 = CIRCLE ( 'NONE', #4732, 1.001129585171333547 ) ;
#339 = CARTESIAN_POINT ( 'NONE',  ( 203.2094460813901833, 24.04198982742622448, -13.33402418452071814 ) ) ;
#340 = VERTEX_POINT ( 'NONE', #1652 ) ;
#341 = LINE ( 'NONE', #19828, #4394 ) ;
#342 = CARTESIAN_POINT ( 'NONE',  ( 76.94659547200038219, 54.56764967722406823, -20.27289619944112786 ) ) ;
#343 = EDGE_CURVE ( 'NONE', #18516, #1461, #6859, .T. ) ;
#345 = ORIENTED_EDGE ( 'NONE', *, *, #6765, .T. ) ;
#344 = ORIENTED_EDGE ( 'NONE', *, *, #7860, .F. ) ;
#346 = VECTOR ( 'NONE', #15320, 1000.000000000000114 ) ;
#347 = ORIENTED_EDGE ( 'NONE', *, *, #464, .T. ) ;
#348 = ADVANCED_FACE ( 'NONE', ( #1860 ), #11088, .F. ) ;
#349 = AXIS2_PLACEMENT_3D ( 'NONE', #19014, #17316, #10832 ) ;
#350 = ORIENTED_EDGE ( 'NONE', *, *, #10318, .F. ) ;
#351 = AXIS2_PLACEMENT_3D ( 'NONE', #10728, #9237, #6058 ) ;
#352 = CARTESIAN_POINT ( 'NONE',  ( 69.50490953756755630, 173.5703347563769796, 16.00000000000001066 ) ) ;
#353 = ORIENTED_EDGE ( 'NONE', *, *, #18968, .F. ) ;
#354 = CARTESIAN_POINT ( 'NONE',  ( 76.60035650392514128, 54.09786888454211606, -5.411621923353880703 ) ) ;
#355 = CARTESIAN_POINT ( 'NONE',  ( -21.06087829250213161, 79.98244021547201044, -11.72107194671396790 ) ) ;
#356 = CARTESIAN_POINT ( 'NONE',  ( 205.5965122587965084, 9.994899983462953941, -14.00000000000005507 ) ) ;
#357 = CARTESIAN_POINT ( 'NONE',  ( 218.1364845712607803, 10.58466899794828642, -8.415281845792092597 ) ) ;
#358 = EDGE_CURVE ( 'NONE', #6609, #4749, #6287, .T. ) ;
#359 = ORIENTED_EDGE ( 'NONE', *, *, #1114, .T. ) ;
#360 = ADVANCED_FACE ( 'NONE', ( #16385 ), #15798, .T. ) ;
#361 = FACE_OUTER_BOUND ( 'NONE', #3551, .T. ) ;
#362 = VECTOR ( 'NONE', #204, 1000.000000000000114 ) ;
#363 = VECTOR ( 'NONE', #26, 1000.000000000000114 ) ;
#364 = CARTESIAN_POINT ( 'NONE',  ( 54.28616200159638083, 77.98283342922744055, -13.21260929400889950 ) ) ;
#365 = CARTESIAN_POINT ( 'NONE',  ( 229.8377178060437132, 36.62479788795283753, -15.02729838650899552 ) ) ;
#366 = ORIENTED_EDGE ( 'NONE', *, *, #15468, .F. ) ;
#367 = AXIS2_PLACEMENT_3D ( 'NONE', #16920, #11953, #10334 ) ;
#369 = EDGE_CURVE ( 'NONE', #14650, #14697, #6503, .T. ) ;
#368 = DIRECTION ( 'NONE',  ( -0.000000000000000000, -1.000000000000000000, -0.000000000000000000 ) ) ;
#370 = LINE ( 'NONE', #11808, #12203 ) ;
#371 = AXIS2_PLACEMENT_3D ( 'NONE', #13826, #2695, #10622 ) ;
#372 = FACE_OUTER_BOUND ( 'NONE', #9443, .T. ) ;
#373 = CARTESIAN_POINT ( 'NONE',  ( -4.811817756148304426, 79.75568800831774752, -9.793444445058595349 ) ) ;
#374 = VECTOR ( 'NONE', #10488, 999.9999999999998863 ) ;
#375 = LINE ( 'NONE', #8408, #1415 ) ;
#376 = EDGE_CURVE ( 'NONE', #7292, #12993, #6301, .T. ) ;
#377 = AXIS2_PLACEMENT_3D ( 'NONE', #5841, #2472, #8925 ) ;
#378 = DIRECTION ( 'NONE',  ( 0.000000000000000000, 0.8660254037844372643, -0.5000000000000024425 ) ) ;
#379 = DIRECTION ( 'NONE',  ( 0.8660254037844371533, 0.5000000000000025535, 0.000000000000000000 ) ) ;
#380 = DIRECTION ( 'NONE',  ( 0.3430151393149036276, 0.1980398830195791438, -0.9182161068802751069 ) ) ;
#381 = ORIENTED_EDGE ( 'NONE', *, *, #17715, .T. ) ;
#382 = AXIS2_PLACEMENT_3D ( 'NONE', #19245, #4714, #11186 ) ;
#383 = CARTESIAN_POINT ( 'NONE',  ( 81.91557740337785276, 60.53556548035048479, -24.72568746032316511 ) ) ;
#384 = FACE_OUTER_BOUND ( 'NONE', #1878, .T. ) ;
#385 = VERTEX_POINT ( 'NONE', #20826 ) ;
#386 = LINE ( 'NONE', #13322, #2071 ) ;
#387 = CARTESIAN_POINT ( 'NONE',  ( -3.556084784758247075, 50.96167829366792290, 1.269699694002965007 ) ) ;
#388 = CARTESIAN_POINT ( 'NONE',  ( -9.537558382401318369, 79.97813440949151698, -11.66361662172994507 ) ) ;
#389 = DIRECTION ( 'NONE',  ( 0.8660254037844355990, 0.5000000000000054401, 0.000000000000000000 ) ) ;
#390 = LINE ( 'NONE', #1771, #19960 ) ;
#391 = CIRCLE ( 'NONE', #14642, 12.00000000000002665 ) ;
#392 = CARTESIAN_POINT ( 'NONE',  ( 205.8264633344831225, 9.596613037118636669, -14.00000000000005507 ) ) ;
#393 = ADVANCED_FACE ( 'NONE', ( #3140 ), #14498, .F. ) ;
#395 = ORIENTED_EDGE ( 'NONE', *, *, #13776, .T. ) ;
#394 = ORIENTED_EDGE ( 'NONE', *, *, #20392, .T. ) ;
#396 = ORIENTED_EDGE ( 'NONE', *, *, #17876, .T. ) ;
#397 = DIRECTION ( 'NONE',  ( -0.8660254037844360431, -0.5000000000000046629, 0.000000000000000000 ) ) ;
#399 = CARTESIAN_POINT ( 'NONE',  ( 77.00490953756757051, 160.5799536996104564, 56.00000000000000711 ) ) ;
#398 = AXIS2_PLACEMENT_3D ( 'NONE', #14212, #20751, #11112 ) ;
#400 = VECTOR ( 'NONE', #17004, 1000.000000000000227 ) ;
#401 = ORIENTED_EDGE ( 'NONE', *, *, #14764, .T. ) ;
#402 = VERTEX_POINT ( 'NONE', #14604 ) ;
#403 = LINE ( 'NONE', #2101, #20013 ) ;
#404 = CARTESIAN_POINT ( 'NONE',  ( 226.0093550869354715, 42.27625073618769846, -11.55788255683058807 ) ) ;
#405 = DIRECTION ( 'NONE',  ( 1.000000000000000000, 0.000000000000000000, 0.000000000000000000 ) ) ;
#406 = ORIENTED_EDGE ( 'NONE', *, *, #11046, .T. ) ;
#407 = CIRCLE ( 'NONE', #12256, 5.999999999999989342 ) ;
#408 = DIRECTION ( 'NONE',  ( -1.000000000000000000, 0.000000000000000000, 0.000000000000000000 ) ) ;
#409 = CARTESIAN_POINT ( 'NONE',  ( -15.99999999999999289, 80.00000000000000000, 0.000000000000000000 ) ) ;
#410 = ORIENTED_EDGE ( 'NONE', *, *, #16561, .T. ) ;
#411 = ADVANCED_FACE ( 'NONE', ( #13000 ), #16084, .T. ) ;
#412 = CARTESIAN_POINT ( 'NONE',  ( 190.8575367324608294, 36.14736977200441004, -19.00000000000003908 ) ) ;
#413 = CIRCLE ( 'NONE', #5471, 12.47473710546057823 ) ;
#414 = B_SPLINE_CURVE_WITH_KNOTS ( 'NONE', 3,
 ( #85, #20834, #6311, #19454 ),
 .UNSPECIFIED., .F., .F.,
 ( 4, 4 ),
 ( 1.346298404090565887E-06, 0.0004533995401839391380 ),
 .UNSPECIFIED. ) ;
#415 = VECTOR ( 'NONE', #6964, 1000.000000000000114 ) ;
#416 = LINE ( 'NONE', #6862, #13294 ) ;
#417 = CARTESIAN_POINT ( 'NONE',  ( -33.37417213237042546, 54.75746433087826404, -1.535552296325748189 ) ) ;
#418 = DIRECTION ( 'NONE',  ( 0.1005394128318083530, 0.05804645706261224447, -0.9932383577419438003 ) ) ;
#419 = VECTOR ( 'NONE', #16683, 999.9999999999998863 ) ;
#420 = CARTESIAN_POINT ( 'NONE',  ( 199.2144802262915846, 21.04890371929339921, -14.00000000000005507 ) ) ;
#421 = DIRECTION ( 'NONE',  ( -0.8660254037844355990, -0.5000000000000054401, 9.734124438199387596E-15 ) ) ;
#422 = EDGE_CURVE ( 'NONE', #16527, #15321, #7895, .T. ) ;
#423 = VERTEX_POINT ( 'NONE', #6399 ) ;
#424 = CARTESIAN_POINT ( 'NONE',  ( 64.92628429094538944, 80.60227088397526529, -21.04771496906974804 ) ) ;
#425 = VERTEX_POINT ( 'NONE', #12897 ) ;
#426 = ORIENTED_EDGE ( 'NONE', *, *, #9003, .F. ) ;
#427 = CARTESIAN_POINT ( 'NONE',  ( 1.500000000000001332, 0.000000000000000000, 0.000000000000000000 ) ) ;
#428 = AXIS2_PLACEMENT_3D ( 'NONE', #10509, #10617, #2589 ) ;
#429 = AXIS2_PLACEMENT_3D ( 'NONE', #15192, #11886, #11994 ) ;
#430 = VECTOR ( 'NONE', #14086, 1000.000000000000114 ) ;
#431 = ORIENTED_EDGE ( 'NONE', *, *, #6280, .F. ) ;
#432 = CARTESIAN_POINT ( 'NONE',  ( 229.4135966341432606, 36.37993141518708740, -15.02729838650899552 ) ) ;
#433 = ITEM_DEFINED_TRANSFORMATION ( 'NONE', 'NONE', #12828,  #18233 ) ;
#434 =( BOUNDED_CURVE ( )  B_SPLINE_CURVE ( 3, ( #6259, #9555, #12753, #12546 ),
 .UNSPECIFIED., .F., .T. ) 
 B_SPLINE_CURVE_WITH_KNOTS ( ( 4, 4 ),
 ( 4.913746901175024107, 6.283185307179586232 ),
 .UNSPECIFIED. ) 
 CURVE ( )  GEOMETRIC_REPRESENTATION_ITEM ( )  RATIONAL_B_SPLINE_CURVE ( ( 1.000000000000000000, 0.8497311128276563430, 0.8497311128276563430, 1.000000000000000000 ) ) 
 REPRESENTATION_ITEM ( '' )  );
#435 = EDGE_CURVE ( 'NONE', #18580, #3050, #17877, .T. ) ;
#436 = CYLINDRICAL_SURFACE ( 'NONE', #19100, 3.902363844300889451 ) ;
#437 = VERTEX_POINT ( 'NONE', #8202 ) ;
#438 = CARTESIAN_POINT ( 'NONE',  ( 212.7108869958215109, 14.10238615300026410, -22.72623880687309139 ) ) ;
#439 = DIRECTION ( 'NONE',  ( 0.000000000000000000, 0.000000000000000000, 1.000000000000000000 ) ) ;
#440 = DIRECTION ( 'NONE',  ( 0.9679941405060923376, 0.000000000000000000, 0.2509727952306220478 ) ) ;
#441 = CARTESIAN_POINT ( 'NONE',  ( 200.5889925535338989, 11.22780505105986748, -1.381056684022586634 ) ) ;
#442 = AXIS2_PLACEMENT_3D ( 'NONE', #5163, #8671, #19692 ) ;
#443 = ADVANCED_FACE ( 'NONE', ( #4623 ), #13103, .F. ) ;
#444 = CARTESIAN_POINT ( 'NONE',  ( 116.4887320753796587, 39.19196698708793747, -12.50000000000000000 ) ) ;
#445 = CARTESIAN_POINT ( 'NONE',  ( 227.5312376355471145, 39.64027283883993391, -14.00000000000005507 ) ) ;
#446 = DIRECTION ( 'NONE',  ( 0.8426815769442687065, 0.4865224352899183979, 0.2306158707424263710 ) ) ;
#447 = ADVANCED_FACE ( 'NONE', ( #5025 ), #888, .T. ) ;
#448 = ORIENTED_EDGE ( 'NONE', *, *, #2524, .T. ) ;
#449 = CYLINDRICAL_SURFACE ( 'NONE', #10512, 3.902363844300889451 ) ;
#450 = CARTESIAN_POINT ( 'NONE',  ( 201.8234976231972553, 26.52995303002162331, -14.00000000000004619 ) ) ;
#451 = CARTESIAN_POINT ( 'NONE',  ( 218.7787453705537928, 10.18265835266665675, -11.24974199967301836 ) ) ;
#452 = CARTESIAN_POINT ( 'NONE',  ( 77.98814704359870120, 52.13394603002385708, -14.43366844821333572 ) ) ;
#454 = ORIENTED_EDGE ( 'NONE', *, *, #14721, .F. ) ;
#453 = EDGE_LOOP ( 'NONE', ( #8064, #10260, #20838, #5288 ) ) ;
#455 = EDGE_CURVE ( 'NONE', #2505, #184, #11818, .T. ) ;
#456 = VERTEX_POINT ( 'NONE', #6830 ) ;
#457 = AXIS2_PLACEMENT_3D ( 'NONE', #2689, #2291, #9232 ) ;
#458 = CARTESIAN_POINT ( 'NONE',  ( 63.15554463217812042, 234.5677573683057062, -19.00000000000000355 ) ) ;
#459 = ORIENTED_EDGE ( 'NONE', *, *, #7794, .F. ) ;
#460 = CARTESIAN_POINT ( 'NONE',  ( 76.86601529753625073, 54.45829969532270809, -4.885926103426701417 ) ) ;
#461 = CARTESIAN_POINT ( 'NONE',  ( -17.30116400286886247, 79.99994664032418257, -12.45114708371502665 ) ) ;
#462 = LINE ( 'NONE', #18261, #4286 ) ;
#463 = CARTESIAN_POINT ( 'NONE',  ( 30.00000000000000355, 5.000000000000000000, 30.00000000000000000 ) ) ;
#464 = EDGE_CURVE ( 'NONE', #15321, #2307, #18152, .T. ) ;
#465 = ORIENTED_EDGE ( 'NONE', *, *, #17085, .T. ) ;
#466 = FACE_OUTER_BOUND ( 'NONE', #2081, .T. ) ;
#467 = EDGE_CURVE ( 'NONE', #12472, #14490, #11407, .T. ) ;
#468 = CARTESIAN_POINT ( 'NONE',  ( 58.42188568717646291, 76.22201287237797374, -19.09002448919735428 ) ) ;
#469 = CARTESIAN_POINT ( 'NONE',  ( 89.99529059433416478, 168.0799536996104848, 21.00000000000000711 ) ) ;
#470 = VERTEX_POINT ( 'NONE', #11931 ) ;
#471 = AXIS2_PLACEMENT_3D ( 'NONE', #2230, #11878, #3809 ) ;
#472 = AXIS2_PLACEMENT_3D ( 'NONE', #20887, #6361, #6670 ) ;
#473 = CARTESIAN_POINT ( 'NONE',  ( 203.1005406747554218, 12.67784803492986434, -27.13030671846408737 ) ) ;
#474 = CARTESIAN_POINT ( 'NONE',  ( 222.1003674505514027, 32.15763657739488224, -15.02729838650899907 ) ) ;
#475 = EDGE_CURVE ( 'NONE', #17447, #7969, #486, .T. ) ;
#476 = CARTESIAN_POINT ( 'NONE',  ( -0.1767699604045824824, 64.25000000000000000, 2.481238266578627449 ) ) ;
#477 = CARTESIAN_POINT ( 'NONE',  ( -3.836698435374707561, 79.99999999983937471, -2.903060217168568435 ) ) ;
#478 = EDGE_CURVE ( 'NONE', #11306, #15921, #11716, .T. ) ;
#480 = EDGE_LOOP ( 'NONE', ( #20277, #17433, #282, #9071 ) ) ;
#479 = ORIENTED_EDGE ( 'NONE', *, *, #14298, .T. ) ;
#481 = ADVANCED_FACE ( 'NONE', ( #18179 ), #19761, .F. ) ;
#482 = LINE ( 'NONE', #19857, #18341 ) ;
#483 = CARTESIAN_POINT ( 'NONE',  ( 1.500000000000001332, 0.000000000000000000, 0.000000000000000000 ) ) ;
#484 = DIRECTION ( 'NONE',  ( 0.5000000000000007772, -0.8660254037844381525, 0.000000000000000000 ) ) ;
#485 = ORIENTED_EDGE ( 'NONE', *, *, #15962, .F. ) ;
#486 = LINE ( 'NONE', #5128, #4264 ) ;
#487 = CARTESIAN_POINT ( 'NONE',  ( -26.66796757275972851, 5.894401750582999533, 6.542839447999508451 ) ) ;
#488 =( LENGTH_UNIT ( ) NAMED_UNIT ( * ) SI_UNIT ( .MILLI., .METRE. ) );
#489 = DIRECTION ( 'NONE',  ( 0.8660254037844352659, 0.5000000000000056621, 0.000000000000000000 ) ) ;
#490 = EDGE_CURVE ( 'NONE', #14308, #10603, #66, .T. ) ;
#491 = VERTEX_POINT ( 'NONE', #4071 ) ;
#492 = CARTESIAN_POINT ( 'NONE',  ( 82.72938175528729232, 60.17526287326926848, -24.94610863806802925 ) ) ;
#493 = CARTESIAN_POINT ( 'NONE',  ( -3.931445803941664430, 46.62695496839331355, -3.273709564003291383 ) ) ;
#494 = ORIENTED_EDGE ( 'NONE', *, *, #20248, .T. ) ;
#495 = FACE_OUTER_BOUND ( 'NONE', #6270, .T. ) ;
#496 = CARTESIAN_POINT ( 'NONE',  ( 0.5172280101801079999, 58.91385993483535799, 1.214474307743183434 ) ) ;
#497 = CARTESIAN_POINT ( 'NONE',  ( 0.4210663660453498047, 78.26446952993892126, -5.493235020936472424 ) ) ;
#498 = EDGE_CURVE ( 'NONE', #3652, #10237, #899, .T. ) ;
#499 = CARTESIAN_POINT ( 'NONE',  ( 105.1989074543211871, 189.2062061502930135, 11.00000000000001066 ) ) ;
#500 = CARTESIAN_POINT ( 'NONE',  ( 97.86136863954072851, 199.4073499008320027, 8.831051211850477145 ) ) ;
#501 = DIRECTION ( 'NONE',  ( -0.000000000000000000, -1.000000000000000000, -0.000000000000000000 ) ) ;
#503 = ORIENTED_EDGE ( 'NONE', *, *, #7221, .T. ) ;
#502 = ORIENTED_EDGE ( 'NONE', *, *, #9754, .F. ) ;
#504 = VERTEX_POINT ( 'NONE', #19028 ) ;
#505 = CIRCLE ( 'NONE', #3203, 0.4000000000000001887 ) ;
#506 = CARTESIAN_POINT ( 'NONE',  ( 226.4161948415057282, 42.55104950179654111, -15.81459191843835654 ) ) ;
#507 = CARTESIAN_POINT ( 'NONE',  ( 218.3021006999761937, 38.11857920074643857, -12.62147488791602790 ) ) ;
#508 = ORIENTED_EDGE ( 'NONE', *, *, #8439, .F. ) ;
#509 = ORIENTED_EDGE ( 'NONE', *, *, #2019, .T. ) ;
#510 = CARTESIAN_POINT ( 'NONE',  ( 78.47145885649602803, 56.68941013563004816, -2.495457786690434610 ) ) ;
#511 = CARTESIAN_POINT ( 'NONE',  ( 226.2091685456994981, 41.93016367357235197, -11.12998660979000931 ) ) ;
#512 = DIRECTION ( 'NONE',  ( -0.4814586436739045072, 0.8339108325863955340, 0.2697967711570115057 ) ) ;
#513 = VERTEX_POINT ( 'NONE', #12564 ) ;
#514 = DIRECTION ( 'NONE',  ( 0.5171545105027486322, 0.2985792958513951434, -0.8021231927550452889 ) ) ;
#515 = CARTESIAN_POINT ( 'NONE',  ( 203.4466382902124622, 1.588261426394339981, -3.504773242918958420 ) ) ;
#516 = EDGE_LOOP ( 'NONE', ( #16773, #17609, #13168, #2183, #18368 ) ) ;
#517 = FACE_OUTER_BOUND ( 'NONE', #17017, .T. ) ;
#518 = CIRCLE ( 'NONE', #2552, 11.94520687646042667 ) ;
#519 = CARTESIAN_POINT ( 'NONE',  ( 5.000000000000000000, 4.685197434473812983, -6.938893903907228378E-15 ) ) ;
#520 = CARTESIAN_POINT ( 'NONE',  ( -32.92944801084382078, 57.01857061577523922, 0.2052755498065614581 ) ) ;
#521 = CARTESIAN_POINT ( 'NONE',  ( 190.7433706042750146, 35.72129598111152404, -19.00000000000003908 ) ) ;
#522 = PLANE ( 'NONE',  #19314 ) ;
#523 = CARTESIAN_POINT ( 'NONE',  ( -31.74999999999995737, 6.123233995736767268E-16, -5.000000000000000888 ) ) ;
#525 = ORIENTED_EDGE ( 'NONE', *, *, #20015, .F. ) ;
#524 = ORIENTED_EDGE ( 'NONE', *, *, #10776, .F. ) ;
#526 = CARTESIAN_POINT ( 'NONE',  ( 54.80454468582367866, 77.76263990853003349, -14.98572519218623889 ) ) ;
#527 = VERTEX_POINT ( 'NONE', #14054 ) ;
#528 = ORIENTED_EDGE ( 'NONE', *, *, #11637, .F. ) ;
#529 = CARTESIAN_POINT ( 'NONE',  ( 26.00000000000000355, 0.000000000000000000, 4.171999999999999709 ) ) ;
#530 = DIRECTION ( 'NONE',  ( -1.000000000000000000, -0.000000000000000000, -0.000000000000000000 ) ) ;
#531 = ORIENTED_EDGE ( 'NONE', *, *, #18795, .T. ) ;
#532 = DIRECTION ( 'NONE',  ( -0.000000000000000000, 1.000000000000000000, -0.000000000000000000 ) ) ;
#533 = AXIS2_PLACEMENT_3D ( 'NONE', #6159, #10536, #10317 ) ;
#534 = DIRECTION ( 'NONE',  ( -0.5000000000000051070, 0.8660254037844359321, -0.000000000000000000 ) ) ;
#535 = ORIENTED_EDGE ( 'NONE', *, *, #9263, .F. ) ;
#536 = EDGE_CURVE ( 'NONE', #19458, #4355, #2580, .T. ) ;
#537 = CARTESIAN_POINT ( 'NONE',  ( 218.1982458705676606, 38.50437924269842682, -13.95848104343157203 ) ) ;
#538 = CARTESIAN_POINT ( 'NONE',  ( 218.7979616150140600, 37.46564110321825325, -11.28015071478337994 ) ) ;
#539 = CARTESIAN_POINT ( 'NONE',  ( 212.9607779367323417, 18.37065867240589156, -8.669480444820855780 ) ) ;
#540 = CARTESIAN_POINT ( 'NONE',  ( 52.00490953756739287, 203.8812238888322383, 16.00000000000001066 ) ) ;
#541 = CARTESIAN_POINT ( 'NONE',  ( 30.10683012259193703, 0.000000000000000000, 0.000000000000000000 ) ) ;
#542 = ORIENTED_EDGE ( 'NONE', *, *, #5514, .T. ) ;
#543 = DIRECTION ( 'NONE',  ( -0.8404609622711977091, 0.000000000000000000, 0.5418720982835085742 ) ) ;
#544 = DIRECTION ( 'NONE',  ( -1.153604387573317816E-16, 8.028960261725416899E-17, -1.000000000000000000 ) ) ;
#545 = PLANE ( 'NONE',  #2441 ) ;
#546 = VECTOR ( 'NONE', #16332, 1000.000000000000114 ) ;
#547 = ORIENTED_EDGE ( 'NONE', *, *, #6024, .F. ) ;
#548 = AXIS2_PLACEMENT_3D ( 'NONE', #2533, #7185, #4221 ) ;
#549 = CARTESIAN_POINT ( 'NONE',  ( 82.83076346201933404, 60.85614612423834302, 0.1131946898860237832 ) ) ;
#550 = CARTESIAN_POINT ( 'NONE',  ( 207.0013954503587286, 3.383002205901548098, -25.76107385416581508 ) ) ;
#551 = CARTESIAN_POINT ( 'NONE',  ( 79.48072094348276551, 49.82842808374601162, -15.22942965609466270 ) ) ;
#552 = B_SPLINE_CURVE_WITH_KNOTS ( 'NONE', 3,
 ( #19683, #19790, #16415, #17907 ),
 .UNSPECIFIED., .F., .F.,
 ( 4, 4 ),
 ( 5.256891072071942815E-05, 0.0007252197027765627845 ),
 .UNSPECIFIED. ) ;
#553 =( BOUNDED_CURVE ( )  B_SPLINE_CURVE ( 3, ( #9239, #19121, #12236, #18698 ),
 .UNSPECIFIED., .F., .F. ) 
 B_SPLINE_CURVE_WITH_KNOTS ( ( 4, 4 ),
 ( 0.000000000000000000, 1.369438406004562347 ),
 .UNSPECIFIED. ) 
 CURVE ( )  GEOMETRIC_REPRESENTATION_ITEM ( )  RATIONAL_B_SPLINE_CURVE ( ( 1.000000000000000000, 0.8497311128276563430, 0.8497311128276563430, 1.000000000000000000 ) ) 
 REPRESENTATION_ITEM ( '' )  );
#554 = ORIENTED_EDGE ( 'NONE', *, *, #4724, .T. ) ;
#555 = VECTOR ( 'NONE', #8498, 999.9999999999998863 ) ;
#556 = ORIENTED_EDGE ( 'NONE', *, *, #2526, .F. ) ;
#557 = ADVANCED_FACE ( 'NONE', ( #8943 ), #5256, .T. ) ;
#558 = PLANE ( 'NONE',  #15135 ) ;
#559 = EDGE_LOOP ( 'NONE', ( #3305, #9040, #19379, #13830, #16196 ) ) ;
#560 = DIRECTION ( 'NONE',  ( 0.000000000000000000, 0.000000000000000000, 1.000000000000000000 ) ) ;
#561 = EDGE_CURVE ( 'NONE', #18877, #3166, #9046, .T. ) ;
#562 = VECTOR ( 'NONE', #12012, 1000.000000000000000 ) ;
#563 = CARTESIAN_POINT ( 'NONE',  ( -26.10629707152433809, 79.63451458383349291, -9.058872303758411348 ) ) ;
#564 = DIRECTION ( 'NONE',  ( -0.8660254037844359321, -0.5000000000000045519, 5.976026924694053325E-17 ) ) ;
#565 = PLANE ( 'NONE',  #13550 ) ;
#566 = VERTEX_POINT ( 'NONE', #1215 ) ;
#567 = DIRECTION ( 'NONE',  ( -0.8660254037844355990, -0.5000000000000054401, 9.734124438199387596E-15 ) ) ;
#568 = FACE_OUTER_BOUND ( 'NONE', #8960, .T. ) ;
#569 = CARTESIAN_POINT ( 'NONE',  ( -30.20545447418457385, 64.25000000000001421, 2.744335235139487406 ) ) ;
#570 = VERTEX_POINT ( 'NONE', #4289 ) ;
#571 =( NAMED_UNIT ( * ) PLANE_ANGLE_UNIT ( ) SI_UNIT ( $, .RADIAN. ) );
#572 = LINE ( 'NONE', #11705, #22 ) ;
#573 = VECTOR ( 'NONE', #13152, 1000.000000000000000 ) ;
#574 = CARTESIAN_POINT ( 'NONE',  ( 205.7612434495831621, 0.2492073957305620258, -14.00000000000005507 ) ) ;
#575 = CARTESIAN_POINT ( 'NONE',  ( -2.600405991085453561, 77.88264414865945184, -4.670285688179051320 ) ) ;
#576 = EDGE_CURVE ( 'NONE', #4996, #3941, #3262, .T. ) ;
#578 = VERTEX_POINT ( 'NONE', #4391 ) ;
#577 = ORIENTED_EDGE ( 'NONE', *, *, #4172, .T. ) ;
#579 = ORIENTED_EDGE ( 'NONE', *, *, #17154, .T. ) ;
#580 = DIRECTION ( 'NONE',  ( 1.000000000000000000, 0.000000000000000000, 0.000000000000000000 ) ) ;
#581 = DIRECTION ( 'NONE',  ( -0.5000000000000051070, 0.8660254037844359321, -0.000000000000000000 ) ) ;
#582 = CARTESIAN_POINT ( 'NONE',  ( 199.2144802262915846, 21.04890371929339921, -14.00000000000005507 ) ) ;
#583 = EDGE_CURVE ( 'NONE', #14019, #631, #10846, .T. ) ;
#584 = CARTESIAN_POINT ( 'NONE',  ( 82.93056326137615031, 61.76632323605970498, -25.30877389655469756 ) ) ;
#585 = CARTESIAN_POINT ( 'NONE',  ( -29.99999999999999645, 5.000000000000000000, 9.729160503328165177 ) ) ;
#586 = CARTESIAN_POINT ( 'NONE',  ( 191.5478494775925640, 36.18576207517880050, -14.00000000000006395 ) ) ;
#587 = ORIENTED_EDGE ( 'NONE', *, *, #10587, .F. ) ;
#588 = CARTESIAN_POINT ( 'NONE',  ( 81.35624441458497813, 64.60845994063853936, -25.49655522582468237 ) ) ;
#589 = EDGE_CURVE ( 'NONE', #17484, #14639, #4503, .T. ) ;
#590 = FACE_OUTER_BOUND ( 'NONE', #6120, .T. ) ;
#591 = EDGE_CURVE ( 'NONE', #18033, #20000, #11388, .T. ) ;
#592 = CIRCLE ( 'NONE', #20223, 6.099999999999999645 ) ;
#593 = ADVANCED_FACE ( 'NONE', ( #20489 ), #18839, .T. ) ;
#594 = CARTESIAN_POINT ( 'NONE',  ( 86.00000000000000000, 65.00000000000000000, -12.50000000000000000 ) ) ;
#595 = CARTESIAN_POINT ( 'NONE',  ( -3.729411824114762020, 52.78418889159976857, -3.786816875109808578 ) ) ;
#596 = LINE ( 'NONE', #6053, #2836 ) ;
#597 = DIRECTION ( 'NONE',  ( 0.5000000000000046629, -0.8660254037844360431, 0.000000000000000000 ) ) ;
#598 = DIRECTION ( 'NONE',  ( -1.000000000000000000, -0.000000000000000000, -0.000000000000000000 ) ) ;
#599 = CARTESIAN_POINT ( 'NONE',  ( 209.9028093415542457, 12.48114176340366122, -13.84394651341481008 ) ) ;
#601 = ORIENTED_EDGE ( 'NONE', *, *, #10960, .T. ) ;
#600 = VERTEX_POINT ( 'NONE', #20184 ) ;
#602 = ORIENTED_EDGE ( 'NONE', *, *, #8700, .T. ) ;
#603 = CARTESIAN_POINT ( 'NONE',  ( 27.66662763442663220, 64.25000000000000000, -1.859747928060467181 ) ) ;
#604 = LINE ( 'NONE', #7163, #17252 ) ;
#605 = ADVANCED_FACE ( 'NONE', ( #2494 ), #17328, .F. ) ;
#606 = ORIENTED_EDGE ( 'NONE', *, *, #5768, .T. ) ;
#607 = ORIENTED_EDGE ( 'NONE', *, *, #16305, .F. ) ;
#608 = AXIS2_PLACEMENT_3D ( 'NONE', #16458, #246, #12770 ) ;
#609 = CARTESIAN_POINT ( 'NONE',  ( 78.05328906524978549, 56.09831538232894843, -3.025823995327162841 ) ) ;
#610 = DIRECTION ( 'NONE',  ( 0.5000000000000049960, -0.8660254037844358210, 0.000000000000000000 ) ) ;
#611 = CARTESIAN_POINT ( 'NONE',  ( 44.00490953756722945, 217.7376303493834087, -14.00000000000002842 ) ) ;
#612 = ORIENTED_EDGE ( 'NONE', *, *, #14481, .T. ) ;
#613 = VECTOR ( 'NONE', #5948, 1000.000000000000114 ) ;
#614 = EDGE_LOOP ( 'NONE', ( #1540, #2040, #6697, #17636 ) ) ;
#615 = CARTESIAN_POINT ( 'NONE',  ( -19.02430517209115735, 70.26110273505831572, -3.991204510516646931 ) ) ;
#616 = EDGE_CURVE ( 'NONE', #631, #3306, #11174, .T. ) ;
#617 = CARTESIAN_POINT ( 'NONE',  ( 227.3848655466122182, 39.89379673368515711, -10.10863206319041296 ) ) ;
#618 = EDGE_CURVE ( 'NONE', #9039, #9755, #2936, .T. ) ;
#619 = VECTOR ( 'NONE', #4263, 1000.000000000000114 ) ;
#620 = CARTESIAN_POINT ( 'NONE',  ( 200.2585560139914378, -0.5099779577875940273, -20.52105855319921801 ) ) ;
#621 = CARTESIAN_POINT ( 'NONE',  ( -28.23075158081314484, 53.16826294859335889, 2.609184450367471708 ) ) ;
#622 = CARTESIAN_POINT ( 'NONE',  ( 199.5722073119862046, -0.9062415656482646353, -8.625373497621064089 ) ) ;
#623 = CARTESIAN_POINT ( 'NONE',  ( 5.000000000000000000, 7.027796151710712813, -4.057500000000007212 ) ) ;
#624 = EDGE_CURVE ( 'NONE', #1467, #8882, #19760, .T. ) ;
#625 = DIRECTION ( 'NONE',  ( -1.000000000000000000, -0.000000000000000000, -0.000000000000000000 ) ) ;
#627 = VERTEX_POINT ( 'NONE', #2705 ) ;
#626 = ORIENTED_EDGE ( 'NONE', *, *, #616, .T. ) ;
#628 = CARTESIAN_POINT ( 'NONE',  ( 55.63769925775388714, 77.40847683933932899, -16.40349017008347587 ) ) ;
#629 = EDGE_CURVE ( 'NONE', #9080, #19592, #13093, .T. ) ;
#630 = EDGE_LOOP ( 'NONE', ( #1633, #10180, #13625, #15445 ) ) ;
#631 = VERTEX_POINT ( 'NONE', #3318 ) ;
#632 = DIRECTION ( 'NONE',  ( 0.8660254037844380415, 0.5000000000000014433, 0.000000000000000000 ) ) ;
#633 = DIRECTION ( 'NONE',  ( 0.8645602258681710506, 0.4991540791356393614, -0.05814482891047953461 ) ) ;
#634 = AXIS2_PLACEMENT_3D ( 'NONE', #2156, #10183, #5206 ) ;
#635 = ORIENTED_EDGE ( 'NONE', *, *, #10307, .F. ) ;
#636 = DIRECTION ( 'NONE',  ( 0.000000000000000000, -0.5746640192525248603, -0.8183894335684777088 ) ) ;
#637 = ORIENTED_EDGE ( 'NONE', *, *, #186, .T. ) ;
#638 = CARTESIAN_POINT ( 'NONE',  ( 218.7676180683545226, 37.51819766771443199, -16.66317149659879249 ) ) ;
#639 = CARTESIAN_POINT ( 'NONE',  ( 30.00000000000000355, 5.000000000000000000, -15.00000000000000000 ) ) ;
#640 = DIRECTION ( 'NONE',  ( -0.8660254037844361541, -0.5000000000000043299, 0.000000000000000000 ) ) ;
#641 = CARTESIAN_POINT ( 'NONE',  ( 226.8903291562342588, 40.75035888801145489, -17.68583624946726474 ) ) ;
#642 = DIRECTION ( 'NONE',  ( -0.7951984747223626027, -0.4591080534401425495, -0.3960797660391542907 ) ) ;
#643 = CARTESIAN_POINT ( 'NONE',  ( 221.8810290428026519, 32.12561167512754423, -13.95848104343170348 ) ) ;
#644 = LINE ( 'NONE', #6991, #11943 ) ;
#645 = EDGE_LOOP ( 'NONE', ( #9924, #18297, #15540 ) ) ;
#646 = CARTESIAN_POINT ( 'NONE',  ( 218.9556298744170135, 35.47312707796260867, -10.49174204642374519 ) ) ;
#647 = FACE_OUTER_BOUND ( 'NONE', #11082, .T. ) ;
#648 = DIRECTION ( 'NONE',  ( -0.8660254037844354880, -0.5000000000000055511, 0.000000000000000000 ) ) ;
#649 = VECTOR ( 'NONE', #3501, 1000.000000000000227 ) ;
#650 = ORIENTED_EDGE ( 'NONE', *, *, #14383, .T. ) ;
#651 = CARTESIAN_POINT ( 'NONE',  ( 79.92501236954103661, 58.85901869437554268, -1.031643761997860897 ) ) ;
#652 = EDGE_CURVE ( 'NONE', #15437, #9266, #15812, .T. ) ;
#653 = ORIENTED_EDGE ( 'NONE', *, *, #12072, .F. ) ;
#654 = CARTESIAN_POINT ( 'NONE',  ( 198.4658173668363190, 5.877991368080599521, -5.291540431471293715 ) ) ;
#655 = CARTESIAN_POINT ( 'NONE',  ( -14.99999999999999645, 0.000000000000000000, -15.00000000000000000 ) ) ;
#657 = ORIENTED_EDGE ( 'NONE', *, *, #13419, .T. ) ;
#656 = ORIENTED_EDGE ( 'NONE', *, *, #14023, .F. ) ;
#658 = FACE_OUTER_BOUND ( 'NONE', #17928, .T. ) ;
#659 = EDGE_LOOP ( 'NONE', ( #1271, #18731 ) ) ;
#660 = CARTESIAN_POINT ( 'NONE',  ( 75.12482142704125465, 52.12498453794043485, -14.42445013263158238 ) ) ;
#661 = CARTESIAN_POINT ( 'NONE',  ( -17.30014261508840434, 80.00000000000054001, -12.43489149392628512 ) ) ;
#662 = FACE_OUTER_BOUND ( 'NONE', #2324, .T. ) ;
#663 = CARTESIAN_POINT ( 'NONE',  ( 220.7506168395117356, 33.87762484391836892, -10.80501622924635186 ) ) ;
#664 = ORIENTED_EDGE ( 'NONE', *, *, #14243, .F. ) ;
#665 = EDGE_CURVE ( 'NONE', #15359, #17948, #14273, .T. ) ;
#666 = B_SPLINE_CURVE_WITH_KNOTS ( 'NONE', 3,
 ( #11011, #4543, #16007, #14102 ),
 .UNSPECIFIED., .F., .F.,
 ( 4, 4 ),
 ( 3.203731838865369014E-05, 0.0005979635406780447289 ),
 .UNSPECIFIED. ) ;
#667 = FACE_OUTER_BOUND ( 'NONE', #13989, .T. ) ;
#668 = AXIS2_PLACEMENT_3D ( 'NONE', #6471, #18619, #19618 ) ;
#669 = LINE ( 'NONE', #15217, #9538 ) ;
#670 = DIRECTION ( 'NONE',  ( 0.8660254037844362651, 0.5000000000000042188, -6.872020471724000490E-17 ) ) ;
#671 = EDGE_LOOP ( 'NONE', ( #12795, #14132, #9579, #15722 ) ) ;
#672 = CARTESIAN_POINT ( 'NONE',  ( 227.5312376355471145, 39.64027283883993391, -14.00000000000005507 ) ) ;
#673 = ADVANCED_FACE ( 'NONE', ( #4999 ), #11280, .F. ) ;
#674 = FACE_OUTER_BOUND ( 'NONE', #15043, .T. ) ;
#675 = EDGE_CURVE ( 'NONE', #11638, #6609, #8654, .T. ) ;
#676 = CARTESIAN_POINT ( 'NONE',  ( 4.000000000000000000, 1.759474945355388398, 3.047499999999996767 ) ) ;
#677 = CONICAL_SURFACE ( 'NONE', #12535, 4.057500000000029416, 1.047197551196593857 ) ;
#678 = DIRECTION ( 'NONE',  ( -1.000000000000000000, -0.000000000000000000, -0.000000000000000000 ) ) ;
#679 = ORIENTED_EDGE ( 'NONE', *, *, #10423, .F. ) ;
#680 = AXIS2_PLACEMENT_3D ( 'NONE', #1042, #9181, #2945 ) ;
#681 = VERTEX_POINT ( 'NONE', #19127 ) ;
#682 = DIRECTION ( 'NONE',  ( -0.000000000000000000, 1.000000000000000000, -0.000000000000000000 ) ) ;
#683 = DIRECTION ( 'NONE',  ( -0.8660254037844360431, -0.5000000000000046629, 0.000000000000000000 ) ) ;
#684 = DIRECTION ( 'NONE',  ( -0.5000000000000049960, 0.8660254037844357100, -0.000000000000000000 ) ) ;
#685 = CARTESIAN_POINT ( 'NONE',  ( 80.96866787924291486, 54.01966784746423400, -21.77093191989936471 ) ) ;
#686 = DIRECTION ( 'NONE',  ( -1.000000000000000000, -0.000000000000000000, -0.000000000000000000 ) ) ;
#687 = DIRECTION ( 'NONE',  ( 0.8660254037844362651, 0.5000000000000043299, 0.000000000000000000 ) ) ;
#688 = VERTEX_POINT ( 'NONE', #7875 ) ;
#689 = AXIS2_PLACEMENT_3D ( 'NONE', #12223, #19001, #18689 ) ;
#690 = CARTESIAN_POINT ( 'NONE',  ( 80.82058163573867660, 65.29640235792498970, -25.49857619709358048 ) ) ;
#691 = VECTOR ( 'NONE', #8828, 1000.000000000000114 ) ;
#692 = CARTESIAN_POINT ( 'NONE',  ( 59.45914026090133575, 84.82127241994479050, -15.89427485249682626 ) ) ;
#693 = VECTOR ( 'NONE', #17106, 1000.000000000000000 ) ;
#694 = VERTEX_POINT ( 'NONE', #14476 ) ;
#695 = LINE ( 'NONE', #805, #4095 ) ;
#696 = CARTESIAN_POINT ( 'NONE',  ( 197.9607918626003311, -1.063772618484184918, -11.13829696442576811 ) ) ;
#697 = AXIS2_PLACEMENT_3D ( 'NONE', #2673, #767, #5401 ) ;
#698 = CARTESIAN_POINT ( 'NONE',  ( 202.6752174627569332, 8.308289646587223132, -25.34310559273323449 ) ) ;
#699 = EDGE_CURVE ( 'NONE', #20505, #17195, #3823, .T. ) ;
#700 = DIRECTION ( 'NONE',  ( -0.8660254037844355990, -0.5000000000000055511, 0.000000000000000000 ) ) ;
#701 = DIRECTION ( 'NONE',  ( 0.000000000000000000, -0.6317949158654976305, 0.7751355909042679793 ) ) ;
#702 = EDGE_CURVE ( 'NONE', #19907, #9631, #6632, .T. ) ;
#704 = ORIENTED_EDGE ( 'NONE', *, *, #7277, .F. ) ;
#703 = ORIENTED_EDGE ( 'NONE', *, *, #15898, .T. ) ;
#705 = EDGE_LOOP ( 'NONE', ( #1909, #17255, #5302, #8140 ) ) ;
#706 = ORIENTED_EDGE ( 'NONE', *, *, #17795, .T. ) ;
#707 = LINE ( 'NONE', #18409, #13248 ) ;
#708 = DIRECTION ( 'NONE',  ( 0.9367698044638429478, 0.000000000000000000, 0.3499461864984006465 ) ) ;
#709 = VECTOR ( 'NONE', #16147, 1000.000000000000000 ) ;
#710 = CIRCLE ( 'NONE', #14277, 13.99999999999999822 ) ;
#711 = EDGE_LOOP ( 'NONE', ( #17334, #865, #11449, #20358 ) ) ;
#712 = ORIENTED_EDGE ( 'NONE', *, *, #4751, .F. ) ;
#713 = CARTESIAN_POINT ( 'NONE',  ( 79.12402306321216372, 57.63706906876117131, -1.778930141804763831 ) ) ;
#714 = CARTESIAN_POINT ( 'NONE',  ( 30.00000000000000355, 0.000000000000000000, -15.00000000000000000 ) ) ;
#715 = VECTOR ( 'NONE', #14881, 1000.000000000000227 ) ;
#716 = DIRECTION ( 'NONE',  ( 0.5000000000000046629, -0.8660254037844360431, -4.006172263299081054E-16 ) ) ;
#717 = ORIENTED_EDGE ( 'NONE', *, *, #18489, .F. ) ;
#718 = AXIS2_PLACEMENT_3D ( 'NONE', #10009, #11737, #18098 ) ;
#719 = ADVANCED_FACE ( 'NONE', ( #9867 ), #20902, .F. ) ;
#720 = DIRECTION ( 'NONE',  ( 0.000000000000000000, 0.000000000000000000, -1.000000000000000000 ) ) ;
#721 = DIRECTION ( 'NONE',  ( 0.5000000000000044409, -0.8660254037844360431, -8.673617379884021914E-17 ) ) ;
#722 = DIRECTION ( 'NONE',  ( 0.5000000000000042188, -0.8660254037844362651, 1.445602896647343847E-16 ) ) ;
#723 = EDGE_CURVE ( 'NONE', #3430, #270, #9321, .T. ) ;
#724 = CIRCLE ( 'NONE', #3436, 3.902363844300875240 ) ;
#725 = CYLINDRICAL_SURFACE ( 'NONE', #12270, 12.50000000000000000 ) ;
#726 = CARTESIAN_POINT ( 'NONE',  ( -15.04600911323590218, 50.47255456144257835, -16.23554317993713170 ) ) ;
#727 = CARTESIAN_POINT ( 'NONE',  ( 209.3139125749813445, 4.975733814115070430, -1.899081834577973860 ) ) ;
#728 = AXIS2_PLACEMENT_3D ( 'NONE', #13100, #4823, #8301 ) ;
#729 = ADVANCED_FACE ( 'NONE', ( #7768 ), #11059, .T. ) ;
#730 = DIRECTION ( 'NONE',  ( -0.1992005449231252778, 0.3450254647022570897, 0.9172113015054499385 ) ) ;
#731 = CONICAL_SURFACE ( 'NONE', #20347, 4.057500000000000107, 1.047197551196593857 ) ;
#732 = DIRECTION ( 'NONE',  ( 0.000000000000000000, -1.000000000000000000, 2.176694594656153859E-16 ) ) ;
#734 = VERTEX_POINT ( 'NONE', #3213 ) ;
#733 = ORIENTED_EDGE ( 'NONE', *, *, #2224, .T. ) ;
#735 = CARTESIAN_POINT ( 'NONE',  ( 60.75134160315762699, 83.82709006120157369, -17.71883169751006548 ) ) ;
#736 = ORIENTED_EDGE ( 'NONE', *, *, #2296, .F. ) ;
#737 = ORIENTED_EDGE ( 'NONE', *, *, #2963, .F. ) ;
#738 = ORIENTED_EDGE ( 'NONE', *, *, #7937, .F. ) ;
#739 = DIRECTION ( 'NONE',  ( -0.000000000000000000, -0.000000000000000000, 1.000000000000000000 ) ) ;
#740 = CYLINDRICAL_SURFACE ( 'NONE', #13407, 5.000000000000005329 ) ;
#741 = B_SPLINE_CURVE_WITH_KNOTS ( 'NONE', 3,
 ( #19475, #14535, #105, #11232 ),
 .UNSPECIFIED., .F., .F.,
 ( 4, 4 ),
 ( 2.042725466720964897E-07, 0.0005856926282862855897 ),
 .UNSPECIFIED. ) ;
#742 = EDGE_CURVE ( 'NONE', #10112, #13861, #2588, .T. ) ;
#743 = VECTOR ( 'NONE', #7557, 1000.000000000000227 ) ;
#744 = EDGE_CURVE ( 'NONE', #6868, #9199, #6180, .T. ) ;
#745 = ORIENTED_EDGE ( 'NONE', *, *, #358, .F. ) ;
#746 = ORIENTED_EDGE ( 'NONE', *, *, #6799, .T. ) ;
#747 = CARTESIAN_POINT ( 'NONE',  ( 218.1639642825640522, 38.35783849407987844, -13.95097276009430587 ) ) ;
#748 = AXIS2_PLACEMENT_3D ( 'NONE', #7309, #8909, #2142 ) ;
#749 = AXIS2_PLACEMENT_3D ( 'NONE', #2905, #7448, #7765 ) ;
#750 = LINE ( 'NONE', #16854, #10405 ) ;
#751 = VECTOR ( 'NONE', #3852, 1000.000000000000227 ) ;
#752 = DIRECTION ( 'NONE',  ( 0.000000000000000000, -0.000000000000000000, -1.000000000000000000 ) ) ;
#753 = FACE_OUTER_BOUND ( 'NONE', #17256, .T. ) ;
#754 = ADVANCED_FACE ( 'NONE', ( #1529, #19230 ), #4696, .F. ) ;
#755 = CARTESIAN_POINT ( 'NONE',  ( 221.0219778807527575, 31.89410734487043442, -14.91677899116122141 ) ) ;
#756 = CARTESIAN_POINT ( 'NONE',  ( 208.8107687779841228, 4.427644383670616079, -14.00000000000005507 ) ) ;
#757 = DIRECTION ( 'NONE',  ( -3.965082230804136925E-15, -7.930164461608273850E-15, 1.000000000000000000 ) ) ;
#758 = ORIENTED_EDGE ( 'NONE', *, *, #19004, .F. ) ;
#759 = CARTESIAN_POINT ( 'NONE',  ( 215.9194406937061217, 8.531838027793467560, -5.321846656828220112 ) ) ;
#760 = DIRECTION ( 'NONE',  ( 0.4988343845952723510, -0.8640064986813598136, -0.06824241336466070618 ) ) ;
#761 = FACE_OUTER_BOUND ( 'NONE', #18990, .T. ) ;
#762 = ORIENTED_EDGE ( 'NONE', *, *, #6271, .T. ) ;
#763 = EDGE_CURVE ( 'NONE', #7000, #12336, #221, .T. ) ;
#764 = VECTOR ( 'NONE', #5969, 1000.000000000000114 ) ;
#765 = CARTESIAN_POINT ( 'NONE',  ( 81.28584910398754459, 61.36302568043885941, -0.01657068726255144647 ) ) ;
#766 = EDGE_LOOP ( 'NONE', ( #3152, #6757, #15999, #10627, #359 ) ) ;
#767 = DIRECTION ( 'NONE',  ( 0.5000000000000054401, -0.8660254037844354880, 0.000000000000000000 ) ) ;
#768 = CARTESIAN_POINT ( 'NONE',  ( 203.1960812450809897, 12.73300840892584063, -0.8632678296711639998 ) ) ;
#769 = CARTESIAN_POINT ( 'NONE',  ( 152.5767063072927954, 13.68576207517851628, -14.00000000000007994 ) ) ;
#770 = VECTOR ( 'NONE', #5873, 1000.000000000000000 ) ;
#771 = CARTESIAN_POINT ( 'NONE',  ( 22.00490953756706958, 255.8427481158984165, 1.000000000000018208 ) ) ;
#772 = VERTEX_POINT ( 'NONE', #13385 ) ;
#773 = CARTESIAN_POINT ( 'NONE',  ( 78.91362683933590461, 57.32445438350235634, -23.00962568793631036 ) ) ;
#774 = CARTESIAN_POINT ( 'NONE',  ( -16.26047902139016088, 79.99999999999998579, -12.49895143242785522 ) ) ;
#775 = CONICAL_SURFACE ( 'NONE', #16675, 4.509097725792825528, 0.5235987755983015912 ) ;
#776 = CARTESIAN_POINT ( 'NONE',  ( 30.00000000000000355, -10.00000000000000000, -28.99999999999999645 ) ) ;
#777 = CARTESIAN_POINT ( 'NONE',  ( 199.3993387870319509, 20.72871929987707063, -14.00000000000005507 ) ) ;
#778 = ORIENTED_EDGE ( 'NONE', *, *, #1234, .T. ) ;
#779 = MECHANICAL_DESIGN_GEOMETRIC_PRESENTATION_REPRESENTATION (  '', ( #4502 ), #19384 ) ;
#780 = CARTESIAN_POINT ( 'NONE',  ( 61.99529059433385925, 216.5773763115390125, -5.999999999999973355 ) ) ;
#781 = CARTESIAN_POINT ( 'NONE',  ( 199.2144802262915846, 21.04890371929339921, -14.00000000000005507 ) ) ;
#782 = CARTESIAN_POINT ( 'NONE',  ( 205.8264633344831225, 9.596613037118636669, -14.00000000000005507 ) ) ;
#783 = PRODUCT ( 'Drill Head Clamping Component', 'Drill Head Clamping Component', '', ( #7533 ) ) ;
#784 = VERTEX_POINT ( 'NONE', #1941 ) ;
#785 = LINE ( 'NONE', #2592, #5078 ) ;
#786 = DIRECTION ( 'NONE',  ( 0.5000000000000051070, -0.8660254037844359321, 0.000000000000000000 ) ) ;
#787 = CARTESIAN_POINT ( 'NONE',  ( 227.9553588074475954, 39.88513931160571957, -14.00000000000005507 ) ) ;
#788 = CARTESIAN_POINT ( 'NONE',  ( -15.47785876946503691, 80.00000332749893062, -12.49385289755957729 ) ) ;
#789 = VECTOR ( 'NONE', #17280, 1000.000000000000227 ) ;
#791 = VERTEX_POINT ( 'NONE', #15207 ) ;
#790 = ORIENTED_EDGE ( 'NONE', *, *, #8700, .F. ) ;
#792 = ORIENTED_EDGE ( 'NONE', *, *, #10046, .T. ) ;
#793 = CARTESIAN_POINT ( 'NONE',  ( 229.3566434666465170, 37.45804308600666843, -11.78314368930809231 ) ) ;
#794 = CARTESIAN_POINT ( 'NONE',  ( 227.9210504938507711, 39.61809397791162723, -17.70769053269357585 ) ) ;
#795 = CARTESIAN_POINT ( 'NONE',  ( 82.80106909841869367, 63.71549435008554241, -25.56184987062727743 ) ) ;
#796 = CARTESIAN_POINT ( 'NONE',  ( -28.50008649836227193, 6.470284334177582863, 0.3892821999670322275 ) ) ;
#797 = FACE_OUTER_BOUND ( 'NONE', #8862, .T. ) ;
#798 = ORIENTED_EDGE ( 'NONE', *, *, #10136, .F. ) ;
#799 = EDGE_CURVE ( 'NONE', #310, #13335, #18256, .T. ) ;
#800 = CARTESIAN_POINT ( 'NONE',  ( 81.32899831459523909, 65.64633111285905898, -25.49135248455479541 ) ) ;
#801 = AXIS2_PLACEMENT_3D ( 'NONE', #9097, #5597, #15294 ) ;
#802 = LINE ( 'NONE', #2502, #12393 ) ;
#803 = VECTOR ( 'NONE', #16193, 1000.000000000000227 ) ;
#804 = VERTEX_POINT ( 'NONE', #19835 ) ;
#805 = CARTESIAN_POINT ( 'NONE',  ( 189.5541235174889607, 15.47149417299831420, -8.415281845791808379 ) ) ;
#806 = CARTESIAN_POINT ( 'NONE',  ( 198.4854721009812124, -1.276069208452816683, -11.19970074074890398 ) ) ;
#807 = DIRECTION ( 'NONE',  ( 0.000000000000000000, 0.000000000000000000, -1.000000000000000000 ) ) ;
#808 = CARTESIAN_POINT ( 'NONE',  ( 96.97892280296886724, 198.7003685781201057, 10.19262075797938749 ) ) ;
#809 = CARTESIAN_POINT ( 'NONE',  ( 200.9478142713745967, -0.1120345173462600208, -21.59012016402711609 ) ) ;
#810 = ORIENTED_EDGE ( 'NONE', *, *, #11877, .F. ) ;
#811 = EDGE_LOOP ( 'NONE', ( #7188, #13971, #15070, #13697 ) ) ;
#812 = CARTESIAN_POINT ( 'NONE',  ( 201.7213150758130382, 0.3345463803147161741, -22.69908973750332848 ) ) ;
#813 = LINE ( 'NONE', #2095, #20345 ) ;
#814 = EDGE_CURVE ( 'NONE', #5086, #6648, #7657, .T. ) ;
#815 = EDGE_LOOP ( 'NONE', ( #10085, #3495, #18007 ) ) ;
#816 = DIRECTION ( 'NONE',  ( 1.000000000000000000, -0.000000000000000000, -0.000000000000000000 ) ) ;
#817 = CARTESIAN_POINT ( 'NONE',  ( 162.0049095375683237, 13.35563505625637859, -19.00000000000000355 ) ) ;
#818 = AXIS2_PLACEMENT_3D ( 'NONE', #8468, #3498, #3698 ) ;
#819 = CIRCLE ( 'NONE', #15126, 14.99999999999999645 ) ;
#820 = LINE ( 'NONE', #20002, #17114 ) ;
#821 = DIRECTION ( 'NONE',  ( -0.8660254037844355990, -0.5000000000000054401, 1.154189040529355901E-14 ) ) ;
#822 = ADVANCED_FACE ( 'NONE', ( #658 ), #1575, .T. ) ;
#823 = EDGE_LOOP ( 'NONE', ( #9472, #292, #20590, #17271 ) ) ;
#824 = EDGE_CURVE ( 'NONE', #14364, #18356, #5520, .T. ) ;
#825 = CARTESIAN_POINT ( 'NONE',  ( -10.99999999999999822, 15.09941697557068530, 0.9999999999999991118 ) ) ;
#826 = DIRECTION ( 'NONE',  ( -0.000000000000000000, -0.000000000000000000, 1.000000000000000000 ) ) ;
#827 = CARTESIAN_POINT ( 'NONE',  ( -17.49467092514650801, 49.50700362264424115, -12.43228238208896030 ) ) ;
#828 = DIRECTION ( 'NONE',  ( 0.000000000000000000, -6.938893903907177533E-18, -1.000000000000000000 ) ) ;
#829 = VECTOR ( 'NONE', #16903, 1000.000000000000000 ) ;
#830 = ORIENTED_EDGE ( 'NONE', *, *, #4106, .F. ) ;
#831 = CARTESIAN_POINT ( 'NONE',  ( 226.0041768852971416, 43.26468553558022023, -14.00000000000005507 ) ) ;
#832 = DIRECTION ( 'NONE',  ( 0.4272097022732502247, -0.7399489098236364804, -0.5195839500354230145 ) ) ;
#833 = EDGE_CURVE ( 'NONE', #12601, #7000, #19833, .T. ) ;
#835 = VERTEX_POINT ( 'NONE', #6798 ) ;
#834 = ORIENTED_EDGE ( 'NONE', *, *, #12337, .F. ) ;
#836 = ORIENTED_EDGE ( 'NONE', *, *, #13762, .F. ) ;
#837 = CARTESIAN_POINT ( 'NONE',  ( 201.9048419744482317, 26.22127161638350756, -13.08418984338544355 ) ) ;
#838 = CARTESIAN_POINT ( 'NONE',  ( 63.10828723790488937, 82.00971617295591898, -19.89823807612492601 ) ) ;
#839 = ORIENTED_EDGE ( 'NONE', *, *, #5529, .T. ) ;
#840 = ORIENTED_EDGE ( 'NONE', *, *, #18761, .T. ) ;
#841 = DIRECTION ( 'NONE',  ( -0.5000000000000049960, 0.8660254037844357100, -0.000000000000000000 ) ) ;
#842 = LINE ( 'NONE', #15284, #12412 ) ;
#843 = EDGE_CURVE ( 'NONE', #19778, #2748, #14999, .T. ) ;
#844 = VERTEX_POINT ( 'NONE', #8603 ) ;
#845 = ORIENTED_EDGE ( 'NONE', *, *, #14471, .T. ) ;
#846 = LINE ( 'NONE', #13785, #16170 ) ;
#847 = ORIENTED_EDGE ( 'NONE', *, *, #1612, .T. ) ;
#848 = ADVANCED_FACE ( 'NONE', ( #20058 ), #558, .F. ) ;
#849 = LINE ( 'NONE', #4134, #8722 ) ;
#850 = CARTESIAN_POINT ( 'NONE',  ( 93.04593889385130012, 210.2557651598135351, 11.00000000000001066 ) ) ;
#851 = CARTESIAN_POINT ( 'NONE',  ( -13.77465266732642846, 19.58876728727312511, 12.30409294039043466 ) ) ;
#852 = ORIENTED_EDGE ( 'NONE', *, *, #12815, .T. ) ;
#853 = DIRECTION ( 'NONE',  ( -0.5000000000000045519, 0.8660254037844361541, 0.000000000000000000 ) ) ;
#854 = CARTESIAN_POINT ( 'NONE',  ( -28.16307471351787228, 76.23982303504115521, 2.898234736985794591 ) ) ;
#855 = CARTESIAN_POINT ( 'NONE',  ( 213.9946316566572193, 7.420549012114688203, -3.662783021451589960 ) ) ;
#856 = EDGE_CURVE ( 'NONE', #7254, #18828, #11586, .T. ) ;
#857 = EDGE_CURVE ( 'NONE', #9189, #14554, #9662, .T. ) ;
#858 = DIRECTION ( 'NONE',  ( 0.1997192025788214198, 0.1153079353712215815, 0.9730448705798235842 ) ) ;
#859 = CARTESIAN_POINT ( 'NONE',  ( 206.8262688097345574, 1.942051447093357419, -14.00000000000005507 ) ) ;
#860 = CARTESIAN_POINT ( 'NONE',  ( 207.0179943350029248, 10.81559304280895262, -12.31324071153516364 ) ) ;
#861 = EDGE_CURVE ( 'NONE', #17088, #19623, #11689, .T. ) ;
#862 = VERTEX_POINT ( 'NONE', #1837 ) ;
#863 = CARTESIAN_POINT ( 'NONE',  ( 81.25108741995337880, 54.86839436850289076, -2.588578014267536975 ) ) ;
#864 = VECTOR ( 'NONE', #2674, 1000.000000000000114 ) ;
#865 = ORIENTED_EDGE ( 'NONE', *, *, #17437, .F. ) ;
#866 = DIRECTION ( 'NONE',  ( 0.5000000000000052180, -0.8660254037844355990, 8.326672684688672821E-17 ) ) ;
#867 = CARTESIAN_POINT ( 'NONE',  ( 4.000000000000000000, 1.759474945355379960, -3.047500000000001652 ) ) ;
#868 = EDGE_CURVE ( 'NONE', #1492, #2398, #16138, .T. ) ;
#869 = DIRECTION ( 'NONE',  ( -0.009692502382575126502, 0.000000000000000000, 0.9999530265955316466 ) ) ;
#870 = LINE ( 'NONE', #1189, #10969 ) ;
#871 = ORIENTED_EDGE ( 'NONE', *, *, #3529, .T. ) ;
#872 = DIRECTION ( 'NONE',  ( -0.8660254037844355990, -0.5000000000000055511, 0.000000000000000000 ) ) ;
#873 = EDGE_CURVE ( 'NONE', #9960, #7294, #7008, .T. ) ;
#874 = LINE ( 'NONE', #4477, #4358 ) ;
#875 = FACE_BOUND ( 'NONE', #4618, .T. ) ;
#876 = CARTESIAN_POINT ( 'NONE',  ( -11.09376813494104397, 14.43059931244999028, 0.9644707416441876680 ) ) ;
#877 = AXIS2_PLACEMENT_3D ( 'NONE', #18226, #14549, #1913 ) ;
#878 = CARTESIAN_POINT ( 'NONE',  ( 202.7409362990318584, 7.815183172608958451, -2.044871543906938705 ) ) ;
#879 = AXIS2_PLACEMENT_3D ( 'NONE', #8903, #12316, #5705 ) ;
#880 = ADVANCED_FACE ( 'NONE', ( #19627 ), #12422, .T. ) ;
#881 = PLANE ( 'NONE',  #5818 ) ;
#882 = ADVANCED_FACE ( 'NONE', ( #16671 ), #18054, .F. ) ;
#883 = FACE_BOUND ( 'NONE', #17859, .T. ) ;
#884 = VERTEX_POINT ( 'NONE', #19733 ) ;
#885 = DIRECTION ( 'NONE',  ( -1.000000000000000000, -0.000000000000000000, -0.000000000000000000 ) ) ;
#886 = DIRECTION ( 'NONE',  ( 0.5000000000000045519, -0.8660254037844359321, 0.000000000000000000 ) ) ;
#887 = ADVANCED_FACE ( 'NONE', ( #5202 ), #10073, .F. ) ;
#888 = CONICAL_SURFACE ( 'NONE', #15470, 4.509097725792825528, 0.5235987755983015912 ) ;
#889 = CARTESIAN_POINT ( 'NONE',  ( 30.10683012259193703, -24.14213562373095456, 0.000000000000000000 ) ) ;
#890 = CARTESIAN_POINT ( 'NONE',  ( -15.47785959468120431, 80.00000000000014211, -12.49180211257053230 ) ) ;
#892 = EDGE_LOOP ( 'NONE', ( #5410, #16325, #18093, #3464, #4447 ) ) ;
#891 = ORIENTED_EDGE ( 'NONE', *, *, #5248, .T. ) ;
#893 = EDGE_LOOP ( 'NONE', ( #12615, #1786 ) ) ;
#894 = AXIS2_PLACEMENT_3D ( 'NONE', #1472, #17166, #19175 ) ;
#895 = CARTESIAN_POINT ( 'NONE',  ( -12.69376962344485449, 11.33472108774821763, 12.05717403569970969 ) ) ;
#896 = CIRCLE ( 'NONE', #4616, 12.47473710546057823 ) ;
#897 = ORIENTED_EDGE ( 'NONE', *, *, #5211, .T. ) ;
#898 = UNCERTAINTY_MEASURE_WITH_UNIT (LENGTH_MEASURE( 1.000000000000000082E-05 ), #14114, 'distance_accuracy_value', 'NONE');
#899 = LINE ( 'NONE', #10964, #14452 ) ;
#900 = CARTESIAN_POINT ( 'NONE',  ( -28.22855330669906593, 8.912322265355541617, 2.677539729764461196 ) ) ;
#901 = ORIENTED_EDGE ( 'NONE', *, *, #17043, .F. ) ;
#902 = LINE ( 'NONE', #18920, #12017 ) ;
#903 = ORIENTED_EDGE ( 'NONE', *, *, #20153, .T. ) ;
#904 = DIRECTION ( 'NONE',  ( -0.5000000000000054401, 0.8660254037844354880, -0.000000000000000000 ) ) ;
#905 = CARTESIAN_POINT ( 'NONE',  ( 205.0662616026534693, 10.91332106064940888, -14.00000000000005507 ) ) ;
#906 = EDGE_LOOP ( 'NONE', ( #13222, #9167, #3814, #3486 ) ) ;
#907 = TOROIDAL_SURFACE ( 'NONE', #12088, 17.50000000000000000, 5.000000000000000000 ) ;
#908 = CARTESIAN_POINT ( 'NONE',  ( 209.6893306017077805, 12.35788975548704016, -15.55404723004300926 ) ) ;
#909 = CARTESIAN_POINT ( 'NONE',  ( 69.50490953756755630, 173.5703347563769796, 6.000000000000010658 ) ) ;
#910 = CARTESIAN_POINT ( 'NONE',  ( 199.2144802262915846, 21.04890371929339921, -14.00000000000005507 ) ) ;
#911 = CARTESIAN_POINT ( 'NONE',  ( 98.22805148513273821, 199.6643403035069753, 8.628462948306966140 ) ) ;
#912 = PLANE ( 'NONE',  #7990 ) ;
#913 = ORIENTED_EDGE ( 'NONE', *, *, #13556, .T. ) ;
#914 = ORIENTED_EDGE ( 'NONE', *, *, #14759, .T. ) ;
#915 = CARTESIAN_POINT ( 'NONE',  ( 211.7316270624183403, 13.53701016684330405, -23.47937149798937995 ) ) ;
#916 = LINE ( 'NONE', #12659, #16572 ) ;
#917 = ORIENTED_EDGE ( 'NONE', *, *, #1703, .T. ) ;
#918 = VERTEX_POINT ( 'NONE', #20154 ) ;
#919 = EDGE_CURVE ( 'NONE', #2330, #10554, #16387, .T. ) ;
#920 = CARTESIAN_POINT ( 'NONE',  ( 205.8264633344831225, 9.596613037118636669, -14.00000000000005507 ) ) ;
#921 = DIRECTION ( 'NONE',  ( -1.000000000000000000, -0.000000000000000000, -0.000000000000000000 ) ) ;
#922 = CARTESIAN_POINT ( 'NONE',  ( 222.0932163834421829, 32.17002258895639244, -12.92165662794200109 ) ) ;
#923 = CARTESIAN_POINT ( 'NONE',  ( 227.3144503281347681, 40.99522536077724766, -17.68583624946726474 ) ) ;
#924 = AXIS2_PLACEMENT_3D ( 'NONE', #4879, #7092, #18654 ) ;
#925 = DIRECTION ( 'NONE',  ( -0.5000000000000054401, 0.8660254037844354880, -0.000000000000000000 ) ) ;
#926 = AXIS2_PLACEMENT_3D ( 'NONE', #11439, #1690, #14540 ) ;
#927 = APPLICATION_CONTEXT ( 'automotive_design' ) ;
#928 = EDGE_LOOP ( 'NONE', ( #19595, #19195, #3468, #19468 ) ) ;
#929 = DIRECTION ( 'NONE',  ( -0.8660254037844363761, -0.5000000000000041078, -0.000000000000000000 ) ) ;
#930 = EDGE_CURVE ( 'NONE', #13861, #1523, #13968, .T. ) ;
#931 = CARTESIAN_POINT ( 'NONE',  ( 228.8082804645358408, 38.40783566665349724, -17.19244756328599522 ) ) ;
#932 = CARTESIAN_POINT ( 'NONE',  ( -14.62719308666609486, 45.60972712416246111, -12.42922832581293413 ) ) ;
#933 = CARTESIAN_POINT ( 'NONE',  ( 218.0696720636782970, 37.00765101952458025, -17.47639052459119569 ) ) ;
#934 = DIRECTION ( 'NONE',  ( -0.8660254037844354880, -0.5000000000000055511, 0.000000000000000000 ) ) ;
#935 = CARTESIAN_POINT ( 'NONE',  ( 25.17200000000003612, 0.000000000000000000, 0.000000000000000000 ) ) ;
#936 = CIRCLE ( 'NONE', #18890, 13.50000000000000711 ) ;
#938 = EDGE_LOOP ( 'NONE', ( #1013, #381, #3588, #9, #15721 ) ) ;
#937 = ORIENTED_EDGE ( 'NONE', *, *, #14366, .F. ) ;
#939 = CARTESIAN_POINT ( 'NONE',  ( 201.8234976231972269, 26.52995303002161620, -13.90027237864162757 ) ) ;
#940 = DIRECTION ( 'NONE',  ( -0.8660254037844355990, -0.5000000000000054401, 1.237624392856779246E-14 ) ) ;
#941 = EDGE_CURVE ( 'NONE', #16685, #4766, #9019, .T. ) ;
#942 = VECTOR ( 'NONE', #9777, 1000.000000000000114 ) ;
#943 = CARTESIAN_POINT ( 'NONE',  ( 57.20986367771971004, 224.8659788670223634, 44.53282986889897899 ) ) ;
#944 = ORIENTED_EDGE ( 'NONE', *, *, #3025, .T. ) ;
#945 = EDGE_CURVE ( 'NONE', #3585, #11939, #6044, .T. ) ;
#946 = ORIENTED_EDGE ( 'NONE', *, *, #6874, .T. ) ;
#947 = PLANE ( 'NONE',  #10845 ) ;
#948 = CARTESIAN_POINT ( 'NONE',  ( -1.752364627967215149, 50.08700668601604633, -10.77852995906744304 ) ) ;
#949 = LINE ( 'NONE', #17067, #3578 ) ;
#950 = VERTEX_POINT ( 'NONE', #7222 ) ;
#951 = VERTEX_POINT ( 'NONE', #2466 ) ;
#952 = FACE_OUTER_BOUND ( 'NONE', #37, .T. ) ;
#953 = ORIENTED_EDGE ( 'NONE', *, *, #3595, .F. ) ;
#954 = DIRECTION ( 'NONE',  ( 0.4711304610594141407, -0.8160218955482504422, -0.3348796121709771700 ) ) ;
#955 = DIRECTION ( 'NONE',  ( 0.5705585702127619063, 0.000000000000000000, 0.8212569134910030488 ) ) ;
#956 = PRODUCT_DEFINITION_SHAPE ( 'NONE', 'NONE',  #20948 ) ;
#957 = CARTESIAN_POINT ( 'NONE',  ( -7.400583024429460366, 65.00000000000000000, -12.50000000000000000 ) ) ;
#958 = VECTOR ( 'NONE', #7619, 999.9999999999998863 ) ;
#959 = CARTESIAN_POINT ( 'NONE',  ( 221.7236785435837021, 32.19223253356614123, -13.56204498775467293 ) ) ;
#960 = FACE_OUTER_BOUND ( 'NONE', #1855, .T. ) ;
#961 = FACE_OUTER_BOUND ( 'NONE', #20565, .T. ) ;
#962 = EDGE_CURVE ( 'NONE', #14228, #10601, #3174, .T. ) ;
#963 = DIRECTION ( 'NONE',  ( 0.3430151393149145633, 0.1980398830195858606, 0.9182161068802694448 ) ) ;
#964 = CARTESIAN_POINT ( 'NONE',  ( 5.000000000000004441, 4.685197434473814759, -6.938893903907228378E-15 ) ) ;
#965 = DIRECTION ( 'NONE',  ( -0.5000000000000031086, 0.8660254037844368202, 0.000000000000000000 ) ) ;
#966 = EDGE_LOOP ( 'NONE', ( #19200, #16679, #7135, #19433, #20564 ) ) ;
#967 = CARTESIAN_POINT ( 'NONE',  ( 80.52543256968870367, 57.14253470624510811, -2.115012055466068741 ) ) ;
#968 = EDGE_CURVE ( 'NONE', #15204, #2259, #12531, .T. ) ;
#969 = ORIENTED_EDGE ( 'NONE', *, *, #20916, .T. ) ;
#970 = VECTOR ( 'NONE', #19207, 1000.000000000000227 ) ;
#971 = ORIENTED_EDGE ( 'NONE', *, *, #18549, .T. ) ;
#972 = DIRECTION ( 'NONE',  ( 0.8296432542242784258, 0.4789947561577511115, 0.2868032327110801583 ) ) ;
#973 = CARTESIAN_POINT ( 'NONE',  ( 79.14338724215045318, 54.34411555289009499, -5.006392671230091906 ) ) ;
#974 = AXIS2_PLACEMENT_3D ( 'NONE', #769, #4260, #2465 ) ;
#975 = APPLICATION_PROTOCOL_DEFINITION ( 'draft international standard', 'automotive_design', 1998, #16373 ) ;
#976 = CARTESIAN_POINT ( 'NONE',  ( 213.4594667654058924, 14.53457888447970170, -21.59012016402729728 ) ) ;
#977 = EDGE_CURVE ( 'NONE', #9718, #6001, #15416, .T. ) ;
#978 = ORIENTED_EDGE ( 'NONE', *, *, #6131, .F. ) ;
#979 = ORIENTED_EDGE ( 'NONE', *, *, #930, .F. ) ;
#980 = CARTESIAN_POINT ( 'NONE',  ( 226.5611656185688787, 41.64699361780763098, -10.90800523708426084 ) ) ;
#981 = CARTESIAN_POINT ( 'NONE',  ( 229.0531201841587574, 37.00429494149224752, -11.55788255683065735 ) ) ;
#982 = CYLINDRICAL_SURFACE ( 'NONE', #9493, 12.47473710546057646 ) ;
#983 = CIRCLE ( 'NONE', #5694, 5.000000000000005329 ) ;
#984 = CARTESIAN_POINT ( 'NONE',  ( 202.6090205221545943, 8.270070825110927615, -2.522505859538386908 ) ) ;
#985 = ADVANCED_FACE ( 'NONE', ( #17194 ), #18683, .F. ) ;
#986 = PRODUCT_DEFINITION_FORMATION_WITH_SPECIFIED_SOURCE ( 'ANY', '', #7367, .NOT_KNOWN. ) ;
#987 = CARTESIAN_POINT ( 'NONE',  ( 219.2382532868116982, 10.96316161069002426, -14.00530714776927255 ) ) ;
#988 = DIRECTION ( 'NONE',  ( 0.3200921998322429629, -0.5544159532159284032, -0.7682212795973754060 ) ) ;
#989 = DIRECTION ( 'NONE',  ( -1.000000000000000000, 0.000000000000000000, 0.000000000000000000 ) ) ;
#990 = ORIENTED_EDGE ( 'NONE', *, *, #7291, .F. ) ;
#991 = PLANE ( 'NONE',  #9815 ) ;
#992 = EDGE_CURVE ( 'NONE', #997, #5249, #4157, .T. ) ;
#993 = CARTESIAN_POINT ( 'NONE',  ( -4.579930894573177369, 68.94695149080686747, 5.083831496961729535 ) ) ;
#994 = B_SPLINE_CURVE_WITH_KNOTS ( 'NONE', 3,
 ( #1011, #15446, #12255, #13953 ),
 .UNSPECIFIED., .F., .F.,
 ( 4, 4 ),
 ( 5.953779341834923750E-07, 0.0004526486197140529083 ),
 .UNSPECIFIED. ) ;
#995 = CARTESIAN_POINT ( 'NONE',  ( 202.7409362990318584, 7.815183172608958451, -2.044871543906938705 ) ) ;
#996 = LINE ( 'NONE', #10624, #19259 ) ;
#998 = ORIENTED_EDGE ( 'NONE', *, *, #19233, .T. ) ;
#997 = VERTEX_POINT ( 'NONE', #771 ) ;
#999 = ORIENTED_EDGE ( 'NONE', *, *, #13447, .F. ) ;
#1000 = VERTEX_POINT ( 'NONE', #976 ) ;
#1001 = AXIS2_PLACEMENT_3D ( 'NONE', #3701, #10052, #11562 ) ;
#1002 = CARTESIAN_POINT ( 'NONE',  ( -15.66959223257168432, 10.09941697557068707, 12.50000000000000000 ) ) ;
#1003 =( LENGTH_UNIT ( ) NAMED_UNIT ( * ) SI_UNIT ( .MILLI., .METRE. ) );
#1004 = ORIENTED_EDGE ( 'NONE', *, *, #4187, .F. ) ;
#1005 = CARTESIAN_POINT ( 'NONE',  ( -26.38519111739858758, 79.82398913006802843, -10.19891841068203142 ) ) ;
#1006 = EDGE_CURVE ( 'NONE', #18042, #12264, #12108, .T. ) ;
#1007 = CARTESIAN_POINT ( 'NONE',  ( -33.99999999999997868, 64.25000000000000000, -2.528164662410438357 ) ) ;
#1008 = EDGE_CURVE ( 'NONE', #18502, #19425, #870, .T. ) ;
#1009 =( LENGTH_UNIT ( ) NAMED_UNIT ( * ) SI_UNIT ( .MILLI., .METRE. ) );
#1010 = DIRECTION ( 'NONE',  ( 0.8660254037844355990, 0.5000000000000054401, 0.000000000000000000 ) ) ;
#1011 = CARTESIAN_POINT ( 'NONE',  ( 218.3021006999761937, 38.11857920074643857, -12.62147488791602790 ) ) ;
#1012 = ADVANCED_FACE ( 'NONE', ( #2576 ), #12330, .F. ) ;
#1013 = ORIENTED_EDGE ( 'NONE', *, *, #3059, .T. ) ;
#1014 = DIRECTION ( 'NONE',  ( 0.4586056507527243031, -0.7943282877419081123, 0.3984010898462484462 ) ) ;
#1015 = DIRECTION ( 'NONE',  ( -0.5000000000000049960, 0.8660254037844357100, -0.000000000000000000 ) ) ;
#1016 = AXIS2_PLACEMENT_3D ( 'NONE', #910, #16815, #20500 ) ;
#1017 = CARTESIAN_POINT ( 'NONE',  ( 219.5483150135131325, 35.03133031408865605, -14.00000000000005507 ) ) ;
#1018 = CARTESIAN_POINT ( 'NONE',  ( 228.3459957934797728, 39.20853620448261978, -17.53429396590399492 ) ) ;
#1019 = DIRECTION ( 'NONE',  ( -3.517351572405780687E-16, 2.595185392108431646E-16, -1.000000000000000000 ) ) ;
#1020 = CIRCLE ( 'NONE', #16932, 3.619616396367202782 ) ;
#1021 = ORIENTED_EDGE ( 'NONE', *, *, #945, .F. ) ;
#1022 = ORIENTED_EDGE ( 'NONE', *, *, #6255, .F. ) ;
#1023 = CARTESIAN_POINT ( 'NONE',  ( 198.8427921854145666, -1.327369585325435697, -11.24974199967268618 ) ) ;
#1024 = EDGE_CURVE ( 'NONE', #3127, #14093, #15053, .T. ) ;
#1025 = ORIENTED_EDGE ( 'NONE', *, *, #12215, .T. ) ;
#1026 = CARTESIAN_POINT ( 'NONE',  ( 74.05523633728022048, 112.6889375482328717, -12.50000000000000000 ) ) ;
#1027 = CARTESIAN_POINT ( 'NONE',  ( 80.02281011973705915, 51.32424184041445159, -6.278812083988356996 ) ) ;
#1028 = CARTESIAN_POINT ( 'NONE',  ( 197.6529114527598381, 5.408659919762685675, -6.286464976498783663 ) ) ;
#1029 = CARTESIAN_POINT ( 'NONE',  ( 205.0662616026534693, 10.91332106064940888, -14.00000000000005507 ) ) ;
#1030 = DIRECTION ( 'NONE',  ( -0.5000000000000053291, 0.8660254037844354880, 0.000000000000000000 ) ) ;
#1031 = CONICAL_SURFACE ( 'NONE', #12883, 11.50000000000002309, 0.7853981633974477239 ) ;
#1032 = VERTEX_POINT ( 'NONE', #14138 ) ;
#1033 = ORIENTED_EDGE ( 'NONE', *, *, #8767, .F. ) ;
#1034 = AXIS2_PLACEMENT_3D ( 'NONE', #19639, #3534, #16472 ) ;
#1035 = LINE ( 'NONE', #20422, #19941 ) ;
#1036 = AXIS2_PLACEMENT_3D ( 'NONE', #3801, #18758, #2222 ) ;
#1037 = SURFACE_SIDE_STYLE ('',( #9278 ) ) ;
#1038 = CARTESIAN_POINT ( 'NONE',  ( -13.06364034290321463, 49.50854601617997020, -12.17427138426762312 ) ) ;
#1039 = FACE_OUTER_BOUND ( 'NONE', #17212, .T. ) ;
#1040 = B_SPLINE_CURVE_WITH_KNOTS ( 'NONE', 3,
 ( #10739, #3012, #12249, #6181 ),
 .UNSPECIFIED., .F., .F.,
 ( 4, 4 ),
 ( 8.181520800398489614E-07, 0.0004528713938599333096 ),
 .UNSPECIFIED. ) ;
#1041 = AXIS2_PLACEMENT_3D ( 'NONE', #13270, #13062, #10059 ) ;
#1042 = CARTESIAN_POINT ( 'NONE',  ( 106.0649328581056210, 189.7062061502930135, 11.00000000000001066 ) ) ;
#1043 = FACE_OUTER_BOUND ( 'NONE', #766, .T. ) ;
#1045 = ORIENTED_EDGE ( 'NONE', *, *, #1095, .T. ) ;
#1044 = EDGE_LOOP ( 'NONE', ( #913, #16767, #17162, #15739, #1155 ) ) ;
#1046 = AXIS2_PLACEMENT_3D ( 'NONE', #11317, #4843, #17688 ) ;
#1047 = LINE ( 'NONE', #7499, #3075 ) ;
#1048 = CARTESIAN_POINT ( 'NONE',  ( 213.0626749079333422, 13.95146441739924725, -5.040853264743544671 ) ) ;
#1049 = CARTESIAN_POINT ( 'NONE',  ( 212.7675431533135679, 7.484909225033065994, -2.551678190571531335 ) ) ;
#1050 = VECTOR ( 'NONE', #11952, 1000.000000000000000 ) ;
#1051 = VERTEX_POINT ( 'NONE', #1087 ) ;
#1052 = ORIENTED_EDGE ( 'NONE', *, *, #9633, .T. ) ;
#1053 = VERTEX_POINT ( 'NONE', #2782 ) ;
#1054 = CARTESIAN_POINT ( 'NONE',  ( -15.99999999999999289, 64.25000000000000000, 0.000000000000000000 ) ) ;
#1055 = DIRECTION ( 'NONE',  ( 0.8660254037844355990, 0.5000000000000054401, 4.449885457462577074E-15 ) ) ;
#1056 = CARTESIAN_POINT ( 'NONE',  ( -31.72276537669240071, 50.43494788623335268, -8.899223764819897298 ) ) ;
#1057 = CARTESIAN_POINT ( 'NONE',  ( 30.10683012259193703, -10.00000000000000000, 5.999999999999998224 ) ) ;
#1058 = ORIENTED_EDGE ( 'NONE', *, *, #9912, .T. ) ;
#1059 = ORIENTED_EDGE ( 'NONE', *, *, #1720, .F. ) ;
#1060 = EDGE_CURVE ( 'NONE', #14979, #11827, #7535, .T. ) ;
#1061 = DIRECTION ( 'NONE',  ( 0.5000000000000055511, -0.8660254037844353769, 2.220446049250313574E-16 ) ) ;
#1062 = VECTOR ( 'NONE', #16123, 1000.000000000000000 ) ;
#1063 = CARTESIAN_POINT ( 'NONE',  ( 209.7467543128910563, 12.39104335059656670, -14.69381062500531954 ) ) ;
#1064 = AXIS2_PLACEMENT_3D ( 'NONE', #3055, #8335, #290 ) ;
#1065 = DIRECTION ( 'NONE',  ( 0.000000000000000000, 0.000000000000000000, 1.000000000000000000 ) ) ;
#1066 = CARTESIAN_POINT ( 'NONE',  ( 10.00000000000000178, 0.000000000000000000, 8.000000000000000000 ) ) ;
#1067 = VECTOR ( 'NONE', #16378, 1000.000000000000227 ) ;
#1068 = EDGE_CURVE ( 'NONE', #5521, #2903, #5936, .T. ) ;
#1069 = CARTESIAN_POINT ( 'NONE',  ( 225.7686324792393293, 43.01970128180838771, -13.96704429371383149 ) ) ;
#1070 = LINE ( 'NONE', #12420, #20824 ) ;
#1071 = DIRECTION ( 'NONE',  ( -0.8660254037844361541, -0.5000000000000045519, -4.336808689942050770E-16 ) ) ;
#1072 = CIRCLE ( 'NONE', #18666, 4.057500000000029416 ) ;
#1073 = CARTESIAN_POINT ( 'NONE',  ( 215.9063259570648654, 8.781865454870326104, -5.186396688528637000 ) ) ;
#1074 = PLANE ( 'NONE',  #8585 ) ;
#1075 = FACE_OUTER_BOUND ( 'NONE', #17462, .T. ) ;
#1076 = ORIENTED_EDGE ( 'NONE', *, *, #18529, .F. ) ;
#1077 = CARTESIAN_POINT ( 'NONE',  ( 75.33430881385784517, 70.41445892100490767, -0.5834797149646978598 ) ) ;
#1078 = AXIS2_PLACEMENT_3D ( 'NONE', #16798, #8628, #10094 ) ;
#1079 = ORIENTED_EDGE ( 'NONE', *, *, #12269, .T. ) ;
#1080 = ORIENTED_EDGE ( 'NONE', *, *, #9660, .F. ) ;
#1081 = CARTESIAN_POINT ( 'NONE',  ( 0.2040382970959897513, 69.52210068921742447, 1.838693167884630109 ) ) ;
#1082 = CARTESIAN_POINT ( 'NONE',  ( 210.7420593526228458, 5.542675516821637949, -26.96550585544247269 ) ) ;
#1083 = AXIS2_PLACEMENT_3D ( 'NONE', #8939, #14269, #20487 ) ;
#1084 = EDGE_CURVE ( 'NONE', #19534, #15457, #5863, .T. ) ;
#1085 = VECTOR ( 'NONE', #6641, 1000.000000000000000 ) ;
#1086 = CONTEXT_DEPENDENT_SHAPE_REPRESENTATION ( #8660, #12478 ) ;
#1087 = CARTESIAN_POINT ( 'NONE',  ( 202.7150726112346319, 7.800250765496993033, -25.94618751764486575 ) ) ;
#1088 = ORIENTED_EDGE ( 'NONE', *, *, #9786, .T. ) ;
#1089 =( NAMED_UNIT ( * ) PLANE_ANGLE_UNIT ( ) SI_UNIT ( $, .RADIAN. ) );
#1090 = CARTESIAN_POINT ( 'NONE',  ( 225.6560297040601313, 42.88822825093131286, -12.92165662794185366 ) ) ;
#1091 = CARTESIAN_POINT ( 'NONE',  ( 105.9489074543212013, 187.9071680446163555, 11.00000000000001066 ) ) ;
#1092 = CARTESIAN_POINT ( 'NONE',  ( 202.0355941508142337, 1.288815579510670828, -24.01557619556968248 ) ) ;
#1093 = EDGE_CURVE ( 'NONE', #8938, #14630, #18997, .T. ) ;
#1094 =( GEOMETRIC_REPRESENTATION_CONTEXT ( 3 ) GLOBAL_UNCERTAINTY_ASSIGNED_CONTEXT ( ( #5747 ) ) GLOBAL_UNIT_ASSIGNED_CONTEXT ( ( #17535, #19424, #17849 ) ) REPRESENTATION_CONTEXT ( 'NONE', 'WORKASPACE' ) );
#1095 = EDGE_CURVE ( 'NONE', #9963, #11917, #13002, .T. ) ;
#1096 = DIRECTION ( 'NONE',  ( 0.8660254037844358210, 0.5000000000000049960, 0.000000000000000000 ) ) ;
#1097 = AXIS2_PLACEMENT_3D ( 'NONE', #19090, #965, #14335 ) ;
#1098 = VECTOR ( 'NONE', #17788, 1000.000000000000114 ) ;
#1099 = VECTOR ( 'NONE', #8346, 1000.000000000000114 ) ;
#1100 = CARTESIAN_POINT ( 'NONE',  ( 203.0861028855985069, 1.895327080324426428, -3.188775577416750995 ) ) ;
#1101 = CARTESIAN_POINT ( 'NONE',  ( 210.8574505745143028, 17.15630205363537186, -5.407152407594056243 ) ) ;
#1102 = CARTESIAN_POINT ( 'NONE',  ( -15.99999999999999289, 0.000000000000000000, 0.000000000000000000 ) ) ;
#1103 = ORIENTED_EDGE ( 'NONE', *, *, #15143, .T. ) ;
#1104 = DIRECTION ( 'NONE',  ( 0.8660254037844352659, 0.5000000000000056621, 0.000000000000000000 ) ) ;
#1105 = CARTESIAN_POINT ( 'NONE',  ( -10.99999999999999822, 15.09941697557068530, 0.9999999999999991118 ) ) ;
#1106 = EDGE_CURVE ( 'NONE', #19041, #17375, #6452, .T. ) ;
#1107 = LINE ( 'NONE', #7760, #18343 ) ;
#1108 = CARTESIAN_POINT ( 'NONE',  ( -15.99999999999999289, 79.99999999999998579, -12.50000000000000000 ) ) ;
#1110 = ORIENTED_EDGE ( 'NONE', *, *, #3916, .F. ) ;
#1109 = ORIENTED_EDGE ( 'NONE', *, *, #16804, .T. ) ;
#1111 = CARTESIAN_POINT ( 'NONE',  ( -14.85679855891570078, 10.22906252849420561, 12.44867321866860266 ) ) ;
#1112 = ORIENTED_EDGE ( 'NONE', *, *, #18437, .T. ) ;
#1113 = AXIS2_PLACEMENT_3D ( 'NONE', #12855, #4784, #4680 ) ;
#1114 = EDGE_CURVE ( 'NONE', #15276, #5187, #16226, .T. ) ;
#1115 = VECTOR ( 'NONE', #8761, 1000.000000000000227 ) ;
#1116 = CARTESIAN_POINT ( 'NONE',  ( 221.5409489109203491, 32.47870473532703528, -12.44819273571347829 ) ) ;
#1117 = DIRECTION ( 'NONE',  ( 1.000000000000000000, 0.000000000000000000, 0.000000000000000000 ) ) ;
#1118 = VECTOR ( 'NONE', #18536, 1000.000000000000114 ) ;
#1119 = SHAPE_REPRESENTATION_RELATIONSHIP ( 'NONE' , 'NONE' ,  #8398, #1482 ) ;
#1120 = CARTESIAN_POINT ( 'NONE',  ( -34.66668267600675080, 65.74999999999997158, 1.813692929321156555 ) ) ;
#1121 = ADVANCED_FACE ( 'NONE', ( #11255 ), #18750, .T. ) ;
#1122 = CARTESIAN_POINT ( 'NONE',  ( 198.4659246047362444, -1.544954184478863901, -13.98474561060102772 ) ) ;
#1123 = ORIENTED_EDGE ( 'NONE', *, *, #8792, .F. ) ;
#1124 = LINE ( 'NONE', #12466, #4797 ) ;
#1125 = CARTESIAN_POINT ( 'NONE',  ( 214.8665333410018263, 15.34694915066777909, -8.609703802792745719 ) ) ;
#1126 = CARTESIAN_POINT ( 'NONE',  ( -14.99999999999999645, 5.000000000000000000, -15.00000000000000000 ) ) ;
#1127 = CIRCLE ( 'NONE', #4512, 7.155882939242646401 ) ;
#1128 = B_SPLINE_CURVE_WITH_KNOTS ( 'NONE', 3,
 ( #9917, #10017, #6633, #8123, #3363, #97, #8337, #16412, #19680, #1576, #5155, #2688, #13233, #6424, #3571, #11641, #3162, #18105, #4852, #11425 ),
 .UNSPECIFIED., .F., .F.,
 ( 4, 2, 2, 2, 2, 2, 2, 2, 2, 4 ),
 ( 0.008555345346386149588, 0.009089294358497906207, 0.009623243370609659356, 0.01069114139483316739, 0.01175903941905667716, 0.01282693744328018692, 0.01389483546750369669, 0.01496273349172720646, 0.01603063151595071623, 0.01709852954017422599 ),
 .UNSPECIFIED. ) ;
#1129 = EDGE_CURVE ( 'NONE', #19322, #784, #1828, .T. ) ;
#1130 = DIRECTION ( 'NONE',  ( -0.8660254037844370423, -0.5000000000000027756, -0.000000000000000000 ) ) ;
#1131 = LINE ( 'NONE', #10862, #20660 ) ;
#1132 = EDGE_CURVE ( 'NONE', #4177, #12009, #16464, .T. ) ;
#1134 = ORIENTED_EDGE ( 'NONE', *, *, #5879, .T. ) ;
#1133 = ORIENTED_EDGE ( 'NONE', *, *, #18363, .F. ) ;
#1135 = VERTEX_POINT ( 'NONE', #6351 ) ;
#1136 = CARTESIAN_POINT ( 'NONE',  ( 218.3033847652179702, 9.908208779213840245, -6.724618537539639007 ) ) ;
#1137 = ORIENTED_EDGE ( 'NONE', *, *, #36, .F. ) ;
#1138 = VERTEX_POINT ( 'NONE', #15927 ) ;
#1139 = CARTESIAN_POINT ( 'NONE',  ( -20.49080202807238393, 12.87717145046493172, 11.66622392198317293 ) ) ;
#1140 = DIRECTION ( 'NONE',  ( -0.4988343845952719624, 0.8640064986813588144, -0.06824241336467461172 ) ) ;
#1141 = DIRECTION ( 'NONE',  ( -0.5000000000000008882, 0.8660254037844381525, 0.000000000000000000 ) ) ;
#1142 = EDGE_CURVE ( 'NONE', #9197, #18033, #6556, .T. ) ;
#1143 = CARTESIAN_POINT ( 'NONE',  ( 198.3196067457501783, -0.8566107491083605474, -18.25196083293855409 ) ) ;
#1144 = PLANE ( 'NONE',  #16507 ) ;
#1145 = TOROIDAL_SURFACE ( 'NONE', #16388, 2.961423854602172501, 1.000000000000000000 ) ;
#1146 = VERTEX_POINT ( 'NONE', #2883 ) ;
#1147 = CARTESIAN_POINT ( 'NONE',  ( 213.7787453705537075, 18.84291239051101741, -11.24974199967302013 ) ) ;
#1148 = EDGE_CURVE ( 'NONE', #3117, #9960, #12846, .T. ) ;
#1149 = LINE ( 'NONE', #9488, #430 ) ;
#1150 = CARTESIAN_POINT ( 'NONE',  ( -26.36906608345258363, 50.04675353776782742, -13.70410848631408385 ) ) ;
#1151 = LINE ( 'NONE', #3896, #18721 ) ;
#1152 = CARTESIAN_POINT ( 'NONE',  ( 199.9308801844630636, -0.4415624623656884684, -20.66514661561410549 ) ) ;
#1153 = CARTESIAN_POINT ( 'NONE',  ( -28.15281455745353512, 46.83340527910446838, -2.943232864391990056 ) ) ;
#1155 = ORIENTED_EDGE ( 'NONE', *, *, #17981, .T. ) ;
#1154 = ORIENTED_EDGE ( 'NONE', *, *, #930, .T. ) ;
#1156 = VECTOR ( 'NONE', #15622, 1000.000000000000000 ) ;
#1157 = CARTESIAN_POINT ( 'NONE',  ( 220.0980799571771058, 35.62570024727892104, -17.89498551959672312 ) ) ;
#1158 = AXIS2_PLACEMENT_3D ( 'NONE', #16759, #2241, #2346 ) ;
#1159 = LINE ( 'NONE', #2642, #11880 ) ;
#1160 = CARTESIAN_POINT ( 'NONE',  ( -3.496475329869574100, 79.99999999992608934, -0.04629550956327706246 ) ) ;
#1161 = ORIENTED_EDGE ( 'NONE', *, *, #19027, .T. ) ;
#1162 = ORIENTED_EDGE ( 'NONE', *, *, #18700, .T. ) ;
#1163 = CARTESIAN_POINT ( 'NONE',  ( 205.3647371392095806, 3.210897180031505371, -25.94618751764486575 ) ) ;
#1164 = LINE ( 'NONE', #1470, #8820 ) ;
#1165 = CARTESIAN_POINT ( 'NONE',  ( 1.088894091976222667, 56.28116656631951997, -0.2880183321277288155 ) ) ;
#1166 = CARTESIAN_POINT ( 'NONE',  ( -28.50046567980698242, 8.570075179949460775, 0.3245954035919153546 ) ) ;
#1167 = ORIENTED_EDGE ( 'NONE', *, *, #13583, .F. ) ;
#1168 = ORIENTED_EDGE ( 'NONE', *, *, #10911, .T. ) ;
#1169 = DIRECTION ( 'NONE',  ( 1.000000000000000000, 0.000000000000000000, 0.000000000000000000 ) ) ;
#1170 = ORIENTED_EDGE ( 'NONE', *, *, #14358, .F. ) ;
#1171 = CARTESIAN_POINT ( 'NONE',  ( 204.2095024616932051, 2.543922127990230209, -25.46066938576250038 ) ) ;
#1172 = FACE_OUTER_BOUND ( 'NONE', #8065, .T. ) ;
#1173 = DIRECTION ( 'NONE',  ( -0.5000000000000047740, 0.8660254037844358210, 0.000000000000000000 ) ) ;
#1174 = CARTESIAN_POINT ( 'NONE',  ( 212.1209189702634035, 13.40774137327457360, -4.128377653168339378 ) ) ;
#1175 = CARTESIAN_POINT ( 'NONE',  ( 226.5880894384074793, 41.60036019391326789, -17.13000457754905170 ) ) ;
#1176 = CARTESIAN_POINT ( 'NONE',  ( 199.1867014016590076, -1.128813506749884343, -18.06789442459577799 ) ) ;
#1177 = CARTESIAN_POINT ( 'NONE',  ( 213.9518117939439890, 7.653426176657557534, -3.504773242919091647 ) ) ;
#1178 = CARTESIAN_POINT ( 'NONE',  ( 26.99999999999999645, 65.00000000000000000, -12.50000000000000000 ) ) ;
#1179 = DIRECTION ( 'NONE',  ( 0.000000000000000000, -0.4999999999999983902, 0.8660254037844394848 ) ) ;
#1180 = FACE_OUTER_BOUND ( 'NONE', #11351, .T. ) ;
#1181 = ORIENTED_EDGE ( 'NONE', *, *, #20493, .T. ) ;
#1182 = CARTESIAN_POINT ( 'NONE',  ( 76.96076175570429712, 69.31984913612060950, -0.1862401116020122038 ) ) ;
#1183 = ORIENTED_EDGE ( 'NONE', *, *, #12632, .F. ) ;
#1184 = EDGE_LOOP ( 'NONE', ( #11879, #20337, #17758, #4615, #18514, #9160 ) ) ;
#1185 = CARTESIAN_POINT ( 'NONE',  ( 227.0694757986931904, 41.41953369233032589, -10.52303454827236884 ) ) ;
#1186 = CARTESIAN_POINT ( 'NONE',  ( 214.4659469037960662, 7.692662996923436580, -2.579136038830254218 ) ) ;
#1187 = EDGE_CURVE ( 'NONE', #10193, #12707, #6084, .T. ) ;
#1188 = PRODUCT_CONTEXT ( 'NONE', #7405, 'mechanical' ) ;
#1189 = CARTESIAN_POINT ( 'NONE',  ( 210.8363079006330452, 5.597089941386081513, -1.053683606938506045 ) ) ;
#1190 = VERTEX_POINT ( 'NONE', #6246 ) ;
#1191 = SURFACE_STYLE_USAGE ( .BOTH. , #7323 ) ;
#1192 = LINE ( 'NONE', #18999, #10771 ) ;
#1193 = FACE_OUTER_BOUND ( 'NONE', #1883, .T. ) ;
#1194 = DIRECTION ( 'NONE',  ( 0.5000000000000057732, -0.8660254037844352659, 4.857225732735059864E-17 ) ) ;
#1195 = DIRECTION ( 'NONE',  ( 0.8660254037844361541, 0.5000000000000043299, -5.976026924694053325E-17 ) ) ;
#1196 = EDGE_CURVE ( 'NONE', #9961, #1291, #4537, .T. ) ;
#1197 = CARTESIAN_POINT ( 'NONE',  ( 206.2111997916997552, 10.34978999605213978, -2.036337243043280676 ) ) ;
#1198 = DIRECTION ( 'NONE',  ( 0.1992005449231190606, -0.3450254647022463761, 0.9172113015054554896 ) ) ;
#1199 = AXIS2_PLACEMENT_3D ( 'NONE', #15525, #15733, #4369 ) ;
#1200 = CYLINDRICAL_SURFACE ( 'NONE', #16859, 5.000000000000033751 ) ;
#1201 = VERTEX_POINT ( 'NONE', #3093 ) ;
#1202 = DIRECTION ( 'NONE',  ( -0.5000000000000045519, 0.8660254037844360431, 0.000000000000000000 ) ) ;
#1203 = FACE_OUTER_BOUND ( 'NONE', #3532, .T. ) ;
#1204 = FACE_OUTER_BOUND ( 'NONE', #16741, .T. ) ;
#1205 = DIRECTION ( 'NONE',  ( 0.4999999999999995004, -0.8660254037844390407, 0.000000000000000000 ) ) ;
#1206 = APPLICATION_CONTEXT ( 'automotive_design' ) ;
#1207 = EDGE_CURVE ( 'NONE', #9907, #14800, #4883, .T. ) ;
#1209 = ORIENTED_EDGE ( 'NONE', *, *, #20082, .F. ) ;
#1208 = VERTEX_POINT ( 'NONE', #4575 ) ;
#1210 = EDGE_CURVE ( 'NONE', #884, #504, #2165, .T. ) ;
#1211 = EDGE_CURVE ( 'NONE', #18631, #5527, #7743, .T. ) ;
#1212 = CARTESIAN_POINT ( 'NONE',  ( -11.26027265087348894, 13.47399565661562626, 11.56734157159816156 ) ) ;
#1213 = DIRECTION ( 'NONE',  ( -0.3841106397986904786, 0.6652991438591134843, -0.6401843996644803747 ) ) ;
#1214 = VECTOR ( 'NONE', #5254, 1000.000000000000227 ) ;
#1215 = CARTESIAN_POINT ( 'NONE',  ( 221.3517569193846271, 32.83641968311255965, -11.78314368930809231 ) ) ;
#1216 = VECTOR ( 'NONE', #2994, 1000.000000000000114 ) ;
#1217 = DIRECTION ( 'NONE',  ( -1.000000000000000000, -0.000000000000000000, -0.000000000000000000 ) ) ;
#1218 = VECTOR ( 'NONE', #4888, 999.9999999999998863 ) ;
#1219 = PLANE ( 'NONE',  #6228 ) ;
#1220 = EDGE_LOOP ( 'NONE', ( #180, #19438, #20677, #16352, #3094, #19216, #16530, #18642, #15744, #18492, #577, #6988, #3840, #11038, #4651 ) ) ;
#1221 = VERTEX_POINT ( 'NONE', #9540 ) ;
#1222 = B_SPLINE_CURVE_WITH_KNOTS ( 'NONE', 3,
 ( #11596, #5310, #18061, #3528 ),
 .UNSPECIFIED., .F., .F.,
 ( 4, 4 ),
 ( 2.122554329699731315E-07, 0.0005857006111725968859 ),
 .UNSPECIFIED. ) ;
#1223 = CARTESIAN_POINT ( 'NONE',  ( 205.5965122587965084, 9.994899983462953941, -14.00000000000005507 ) ) ;
#1224 = VERTEX_POINT ( 'NONE', #14553 ) ;
#1225 = DIRECTION ( 'NONE',  ( 0.000000000000000000, 0.000000000000000000, -1.000000000000000000 ) ) ;
#1226 = LINE ( 'NONE', #7675, #19537 ) ;
#1227 = EDGE_CURVE ( 'NONE', #14364, #279, #19497, .T. ) ;
#1228 = CARTESIAN_POINT ( 'NONE',  ( 203.7831613941889088, 8.947961373646505123, -25.80036831778739881 ) ) ;
#1229 = CARTESIAN_POINT ( 'NONE',  ( 10.49211908931699178, -24.14213562373095456, 0.000000000000000000 ) ) ;
#1230 = CIRCLE ( 'NONE', #1557, 4.057500000000000107 ) ;
#1231 = VERTEX_POINT ( 'NONE', #10934 ) ;
#1232 = AXIS2_PLACEMENT_3D ( 'NONE', #4635, #11100, #8006 ) ;
#1233 = FACE_BOUND ( 'NONE', #5689, .T. ) ;
#1234 = EDGE_CURVE ( 'NONE', #10655, #15958, #18417, .T. ) ;
#1235 = ORIENTED_EDGE ( 'NONE', *, *, #18795, .F. ) ;
#1236 = ORIENTED_EDGE ( 'NONE', *, *, #11597, .T. ) ;
#1237 = CARTESIAN_POINT ( 'NONE',  ( 220.3939543724086718, 34.70130055889879372, -10.38579831631093953 ) ) ;
#1238 = DIRECTION ( 'NONE',  ( 0.5000000000000051070, -0.8660254037844359321, 0.000000000000000000 ) ) ;
#1239 = LINE ( 'NONE', #15772, #8678 ) ;
#1240 = EDGE_CURVE ( 'NONE', #12009, #12098, #10909, .T. ) ;
#1241 = CARTESIAN_POINT ( 'NONE',  ( 209.9776323673034426, 12.17031427610509908, -2.697891510991576869 ) ) ;
#1242 = PRESENTATION_STYLE_ASSIGNMENT (( #4414 ) ) ;
#1243 = ADVANCED_FACE ( 'NONE', ( #20676 ), #436, .T. ) ;
#1244 = AXIS2_PLACEMENT_3D ( 'NONE', #5646, #18600, #13730 ) ;
#1245 = ORIENTED_EDGE ( 'NONE', *, *, #4758, .T. ) ;
#1246 = EDGE_CURVE ( 'NONE', #6296, #7157, #7592, .T. ) ;
#1247 = AXIS2_PLACEMENT_3D ( 'NONE', #3781, #10338, #3669 ) ;
#1248 = CARTESIAN_POINT ( 'NONE',  ( 196.9311089575304266, 4.991927054840251010, -20.59651891138145174 ) ) ;
#1249 = CARTESIAN_POINT ( 'NONE',  ( 210.7957517463719057, 12.99668230119596934, -3.627429155984617459 ) ) ;
#1250 = CARTESIAN_POINT ( 'NONE',  ( -11.24740156498038779, 50.36046179987343407, -15.77731508861108445 ) ) ;
#1251 = FACE_OUTER_BOUND ( 'NONE', #16643, .T. ) ;
#1252 = EDGE_CURVE ( 'NONE', #8980, #17374, #4189, .T. ) ;
#1253 = DIRECTION ( 'NONE',  ( -0.5000000000000008882, 0.8660254037844381525, 0.000000000000000000 ) ) ;
#1254 = CARTESIAN_POINT ( 'NONE',  ( -21.23833354872890311, 45.29156160041301860, -11.37540731453001541 ) ) ;
#1256 = ORIENTED_EDGE ( 'NONE', *, *, #17820, .F. ) ;
#1255 = ORIENTED_EDGE ( 'NONE', *, *, #14078, .T. ) ;
#1257 = CARTESIAN_POINT ( 'NONE',  ( -15.99999999999999289, 15.09941697557068530, 0.9999999999999991118 ) ) ;
#1258 = CARTESIAN_POINT ( 'NONE',  ( -25.99999999999999645, 9.999999999999994671, 7.500000000000000000 ) ) ;
#1259 = CARTESIAN_POINT ( 'NONE',  ( 37.00490953756720813, 229.8619860023653132, 26.00000000000001776 ) ) ;
#1260 = ORIENTED_EDGE ( 'NONE', *, *, #15399, .F. ) ;
#1261 = ORIENTED_EDGE ( 'NONE', *, *, #6861, .T. ) ;
#1262 = AXIS2_PLACEMENT_3D ( 'NONE', #9740, #1916, #8362 ) ;
#1263 = FACE_OUTER_BOUND ( 'NONE', #4142, .T. ) ;
#1264 = AXIS2_PLACEMENT_3D ( 'NONE', #6030, #17709, #18980 ) ;
#1265 = DIRECTION ( 'NONE',  ( -1.000000000000000000, 0.000000000000000000, 0.000000000000000000 ) ) ;
#1266 = CARTESIAN_POINT ( 'NONE',  ( -31.04127923955400803, 50.23417253100409852, -9.842805686593695924 ) ) ;
#1267 = EDGE_CURVE ( 'NONE', #13023, #3226, #5866, .T. ) ;
#1268 = PLANE ( 'NONE',  #18508 ) ;
#1269 = ADVANCED_FACE ( 'NONE', ( #16339 ), #11667, .T. ) ;
#1270 = ORIENTED_EDGE ( 'NONE', *, *, #3290, .T. ) ;
#1271 = ORIENTED_EDGE ( 'NONE', *, *, #5205, .T. ) ;
#1272 = CARTESIAN_POINT ( 'NONE',  ( 219.5098200550326908, 36.43861821987845673, -17.58494696003837987 ) ) ;
#1273 = ADVANCED_FACE ( 'NONE', ( #7094 ), #3386, .T. ) ;
#1274 = DIRECTION ( 'NONE',  ( 0.000000000000000000, 0.000000000000000000, 1.000000000000000000 ) ) ;
#1275 = DIRECTION ( 'NONE',  ( 0.8660254037844369313, 0.5000000000000027756, 0.000000000000000000 ) ) ;
#1276 = EDGE_CURVE ( 'NONE', #12454, #9370, #18344, .T. ) ;
#1277 = LINE ( 'NONE', #9721, #2686 ) ;
#1278 = DIRECTION ( 'NONE',  ( 0.000000000000000000, 0.000000000000000000, 1.000000000000000000 ) ) ;
#1279 = CIRCLE ( 'NONE', #13122, 12.47473710546057823 ) ;
#1280 = CARTESIAN_POINT ( 'NONE',  ( 226.4168824216490918, 41.57039268699056578, -17.20332536629370068 ) ) ;
#1281 = CARTESIAN_POINT ( 'NONE',  ( -27.88482465330859839, 73.88542888634933092, 3.878668165723263339 ) ) ;
#1282 = CARTESIAN_POINT ( 'NONE',  ( -20.33207080104639530, 17.61692987535746369, 11.72687972142948709 ) ) ;
#1283 = EDGE_CURVE ( 'NONE', #13189, #11638, #14723, .T. ) ;
#1284 = AXIS2_PLACEMENT_3D ( 'NONE', #20720, #9259, #6188 ) ;
#1285 = CARTESIAN_POINT ( 'NONE',  ( -28.65129735818244683, 65.53858748455373018, 2.490407514064852723 ) ) ;
#1286 = CARTESIAN_POINT ( 'NONE',  ( 219.1740455332299007, 36.81424464895889770, -17.25078732088837086 ) ) ;
#1287 = CARTESIAN_POINT ( 'NONE',  ( 4.000000000000000000, 5.278424836066145431, -3.047500000000006093 ) ) ;
#1288 = VERTEX_POINT ( 'NONE', #3599 ) ;
#1289 = CARTESIAN_POINT ( 'NONE',  ( 71.98518577010987940, 75.06736630765306018, -1.005590943479974131 ) ) ;
#1290 = ORIENTED_EDGE ( 'NONE', *, *, #8492, .F. ) ;
#1291 = VERTEX_POINT ( 'NONE', #4976 ) ;
#1292 = CARTESIAN_POINT ( 'NONE',  ( 30.10683012259193703, -10.00000000000000000, -5.999999999999998224 ) ) ;
#1293 = CARTESIAN_POINT ( 'NONE',  ( -14.99999999999999822, 0.000000000000000000, -28.99999999999999645 ) ) ;
#1294 = ADVANCED_FACE ( 'NONE', ( #13363 ), #10150, .T. ) ;
#1295 = PRESENTATION_LAYER_ASSIGNMENT (  '', '', ( #14167 ) ) ;
#1296 = VECTOR ( 'NONE', #4686, 1000.000000000000227 ) ;
#1297 = CARTESIAN_POINT ( 'NONE',  ( 229.5611158381729240, 36.45092741727606267, -13.51412976915892550 ) ) ;
#1298 = ORIENTED_EDGE ( 'NONE', *, *, #15859, .T. ) ;
#1299 = DIRECTION ( 'NONE',  ( -0.5000000000000047740, 0.8660254037844358210, 0.000000000000000000 ) ) ;
#1300 = CARTESIAN_POINT ( 'NONE',  ( 210.6607590550263183, 28.44678604684768786, -16.18447207777755281 ) ) ;
#1301 = LINE ( 'NONE', #20263, #5405 ) ;
#1302 = FACE_OUTER_BOUND ( 'NONE', #1876, .T. ) ;
#1303 = DIRECTION ( 'NONE',  ( -0.000000000000000000, -1.000000000000000000, -0.000000000000000000 ) ) ;
#1304 = DIRECTION ( 'NONE',  ( 0.8660254037844352659, 0.5000000000000056621, 0.000000000000000000 ) ) ;
#1305 = DIRECTION ( 'NONE',  ( 0.5000000000000044409, -0.8660254037844360431, 0.000000000000000000 ) ) ;
#1306 = EDGE_CURVE ( 'NONE', #694, #5859, #19492, .T. ) ;
#1307 = DIRECTION ( 'NONE',  ( -0.8660254037844377084, -0.5000000000000017764, 0.000000000000000000 ) ) ;
#1308 = ORIENTED_EDGE ( 'NONE', *, *, #2161, .F. ) ;
#1309 = CARTESIAN_POINT ( 'NONE',  ( -7.400583024429460366, 65.00000000000000000, -2.500000000000005773 ) ) ;
#1310 = DIRECTION ( 'NONE',  ( -1.000000000000000000, -0.000000000000000000, -0.000000000000000000 ) ) ;
#1311 = DIRECTION ( 'NONE',  ( 0.5000000000000046629, -0.8660254037844360431, -4.006172263299081054E-16 ) ) ;
#1312 = LINE ( 'NONE', #10835, #6469 ) ;
#1313 = DIRECTION ( 'NONE',  ( 0.5000000000000055511, -0.8660254037844353769, -3.885780586188047891E-16 ) ) ;
#1315 = ORIENTED_EDGE ( 'NONE', *, *, #3282, .F. ) ;
#1314 = ORIENTED_EDGE ( 'NONE', *, *, #8642, .T. ) ;
#1316 = ORIENTED_EDGE ( 'NONE', *, *, #3981, .F. ) ;
#1317 = LINE ( 'NONE', #10841, #8842 ) ;
#1318 = CARTESIAN_POINT ( 'NONE',  ( -35.00000000000000000, 65.00000000000000000, -27.49999999999999645 ) ) ;
#1319 = PRODUCT_DEFINITION_CONTEXT ( 'detailed design', #13525, 'design' ) ;
#1320 = EDGE_CURVE ( 'NONE', #8085, #4151, #16435, .T. ) ;
#1321 = DIRECTION ( 'NONE',  ( -0.8660254037844364872, -0.5000000000000041078, 0.000000000000000000 ) ) ;
#1322 = CIRCLE ( 'NONE', #9753, 15.00000000000000000 ) ;
#1323 = DIRECTION ( 'NONE',  ( 0.000000000000000000, -6.938893903907177533E-18, -1.000000000000000000 ) ) ;
#1324 = DIRECTION ( 'NONE',  ( 0.1997192025788090408, 0.1153079353712143929, -0.9730448705798271369 ) ) ;
#1325 = PRODUCT_DEFINITION_FORMATION_WITH_SPECIFIED_SOURCE ( 'ANY', '', #20237, .NOT_KNOWN. ) ;
#1326 = CARTESIAN_POINT ( 'NONE',  ( 226.2417130873235465, 42.85326076503381643, -12.98880265512658561 ) ) ;
#1327 = DIRECTION ( 'NONE',  ( 0.000000000000000000, 0.000000000000000000, 1.000000000000000000 ) ) ;
#1328 = VERTEX_POINT ( 'NONE', #16749 ) ;
#1329 = DIRECTION ( 'NONE',  ( -0.8137976813493730255, -0.4698463103929600426, -0.3420201433256623291 ) ) ;
#1330 = EDGE_CURVE ( 'NONE', #7157, #3143, #8364, .T. ) ;
#1331 = CARTESIAN_POINT ( 'NONE',  ( 5.000000000000000000, -2.342598717236899386, 4.057500000000001883 ) ) ;
#1332 = DIRECTION ( 'NONE',  ( 0.000000000000000000, 0.000000000000000000, -1.000000000000000000 ) ) ;
#1333 = DIRECTION ( 'NONE',  ( 0.3155439721630258765, -0.5465381918084566415, 0.7757112907044233507 ) ) ;
#1334 = VECTOR ( 'NONE', #3601, 1000.000000000000114 ) ;
#1335 = ORIENTED_EDGE ( 'NONE', *, *, #16418, .T. ) ;
#1336 = FACE_OUTER_BOUND ( 'NONE', #14267, .T. ) ;
#1337 = VERTEX_POINT ( 'NONE', #16647 ) ;
#1338 = ORIENTED_EDGE ( 'NONE', *, *, #16161, .T. ) ;
#1339 = CARTESIAN_POINT ( 'NONE',  ( 203.3234976231972553, 23.93187681866832861, -14.00000000000004441 ) ) ;
#1340 = LINE ( 'NONE', #16082, #15648 ) ;
#1341 = DIRECTION ( 'NONE',  ( 0.8660254037844360431, 0.5000000000000044409, 4.336808689942049290E-16 ) ) ;
#1342 = B_SPLINE_CURVE_WITH_KNOTS ( 'NONE', 3,
 ( #15658, #12259, #12363, #1125 ),
 .UNSPECIFIED., .F., .F.,
 ( 4, 4 ),
 ( 6.919709117056541925E-07, 0.0006733427629548835750 ),
 .UNSPECIFIED. ) ;
#1343 = PLANE ( 'NONE',  #10342 ) ;
#1344 = CARTESIAN_POINT ( 'NONE',  ( 217.5814590494791787, 37.85326076503379511, -12.98880265512657850 ) ) ;
#1345 = VERTEX_POINT ( 'NONE', #2130 ) ;
#1346 = AXIS2_PLACEMENT_3D ( 'NONE', #11621, #3550, #9993 ) ;
#1347 = CARTESIAN_POINT ( 'NONE',  ( 215.7735982840993927, 15.87064333973761343, -15.39542905462748656 ) ) ;
#1348 = ADVANCED_FACE ( 'NONE', ( #8581 ), #10797, .F. ) ;
#1349 = CONICAL_SURFACE ( 'NONE', #17952, 38.65920715899539317, 0.03863996524032856789 ) ;
#1350 = EDGE_CURVE ( 'NONE', #14490, #14969, #12086, .T. ) ;
#1351 =( NAMED_UNIT ( * ) SI_UNIT ( $, .STERADIAN. ) SOLID_ANGLE_UNIT ( ) );
#1352 = CARTESIAN_POINT ( 'NONE',  ( -4.908256850829183726, 51.34256347499046313, -6.001213154916446690 ) ) ;
#1353 = CARTESIAN_POINT ( 'NONE',  ( -15.99999999999999289, 5.000000000000000000, 0.000000000000000000 ) ) ;
#1354 = CONICAL_SURFACE ( 'NONE', #14567, 4.172000000000029907, 0.7853981633974425058 ) ;
#1355 = FACE_OUTER_BOUND ( 'NONE', #13439, .T. ) ;
#1356 = CARTESIAN_POINT ( 'NONE',  ( 96.89336873520835525, 198.6246579379146340, 11.32949238779788637 ) ) ;
#1357 = ORIENTED_EDGE ( 'NONE', *, *, #337, .T. ) ;
#1358 = CARTESIAN_POINT ( 'NONE',  ( 76.19073749086850000, 131.9901410505959518, 41.00000000000001421 ) ) ;
#1359 = CARTESIAN_POINT ( 'NONE',  ( 212.7272071507568967, 14.11180859884542649, -5.291540431471497996 ) ) ;
#1360 =( NAMED_UNIT ( * ) SI_UNIT ( $, .STERADIAN. ) SOLID_ANGLE_UNIT ( ) );
#1361 = ORIENTED_EDGE ( 'NONE', *, *, #4420, .F. ) ;
#1362 = EDGE_LOOP ( 'NONE', ( #19782, #2741, #18153, #20632 ) ) ;
#1363 = EDGE_CURVE ( 'NONE', #4599, #1597, #19419, .T. ) ;
#1364 = VERTEX_POINT ( 'NONE', #7201 ) ;
#1365 = CARTESIAN_POINT ( 'NONE',  ( 57.00490953756744972, 195.2209698509878990, 11.00000000000001066 ) ) ;
#1366 = CARTESIAN_POINT ( 'NONE',  ( 200.7657312721003393, 22.45514972733838732, -14.00000000000005507 ) ) ;
#1367 = CARTESIAN_POINT ( 'NONE',  ( -3.506621468774197670, 49.99927930435590184, -12.32165535527945721 ) ) ;
#1368 = DIRECTION ( 'NONE',  ( 0.000000000000000000, -0.4999999999999985012, 0.8660254037844394848 ) ) ;
#1369 = EDGE_LOOP ( 'NONE', ( #13585, #2991, #15137 ) ) ;
#1370 = CIRCLE ( 'NONE', #10141, 5.999999999999998224 ) ;
#1371 = ORIENTED_EDGE ( 'NONE', *, *, #1850, .F. ) ;
#1372 = DIRECTION ( 'NONE',  ( 0.000000000000000000, 0.000000000000000000, -1.000000000000000000 ) ) ;
#1373 = ADVANCED_FACE ( 'NONE', ( #1172 ), #20136, .F. ) ;
#1374 = DIRECTION ( 'NONE',  ( -0.2300325188655793496, 0.3984280100682197068, -0.8878852184023763305 ) ) ;
#1375 = AXIS2_PLACEMENT_3D ( 'NONE', #11461, #17835, #16236 ) ;
#1376 = EDGE_CURVE ( 'NONE', #17532, #14523, #18555, .T. ) ;
#1377 = DIRECTION ( 'NONE',  ( -0.5000000000000049960, 0.8660254037844358210, -0.000000000000000000 ) ) ;
#1378 = CARTESIAN_POINT ( 'NONE',  ( 207.8614403295549380, 4.652369439064019119, -1.545471579934808215 ) ) ;
#1379 = CARTESIAN_POINT ( 'NONE',  ( 61.57468973143931379, 74.87077495648827608, -20.95977551465544764 ) ) ;
#1380 = AXIS2_PLACEMENT_3D ( 'NONE', #19536, #19849, #3737 ) ;
#1381 = ORIENTED_EDGE ( 'NONE', *, *, #20614, .T. ) ;
#1382 = CARTESIAN_POINT ( 'NONE',  ( -29.99999999999999645, 5.000000000000000000, 10.50000000000000000 ) ) ;
#1383 = VECTOR ( 'NONE', #9881, 1000.000000000000000 ) ;
#1384 = CARTESIAN_POINT ( 'NONE',  ( 208.4761278624580711, 5.007259451653140125, -14.00000000000005507 ) ) ;
#1385 = CYLINDRICAL_SURFACE ( 'NONE', #18691, 3.902363844300889451 ) ;
#1386 = EDGE_LOOP ( 'NONE', ( #16247, #3887, #7387, #1033, #8752, #6624 ) ) ;
#1387 = CARTESIAN_POINT ( 'NONE',  ( 77.64194032647326082, 70.38417867298623776, 0.2137292797775141029 ) ) ;
#1388 = VECTOR ( 'NONE', #2434, 1000.000000000000000 ) ;
#1389 = EDGE_CURVE ( 'NONE', #2300, #18834, #20107, .T. ) ;
#1390 = ORIENTED_EDGE ( 'NONE', *, *, #8484, .T. ) ;
#1391 = EDGE_CURVE ( 'NONE', #6871, #9451, #11642, .T. ) ;
#1392 = ORIENTED_EDGE ( 'NONE', *, *, #8590, .F. ) ;
#1393 = CARTESIAN_POINT ( 'NONE',  ( -4.294235668597638167, 72.30161019875538386, 4.406123080991324770 ) ) ;
#1394 = AXIS2_PLACEMENT_3D ( 'NONE', #12521, #7732, #16494 ) ;
#1395 = AXIS2_PLACEMENT_3D ( 'NONE', #15366, #5459, #20105 ) ;
#1396 = CARTESIAN_POINT ( 'NONE',  ( -24.67152222510459580, 79.91873556435304238, -10.93282151138175173 ) ) ;
#1397 = VECTOR ( 'NONE', #12970, 1000.000000000000000 ) ;
#1398 = ADVANCED_FACE ( 'NONE', ( #10473 ), #4344, .T. ) ;
#1399 = AXIS2_PLACEMENT_3D ( 'NONE', #17157, #2641, #9082 ) ;
#1400 = DIRECTION ( 'NONE',  ( -0.000000000000000000, -1.000000000000000000, 1.117161918529055486E-15 ) ) ;
#1401 = ORIENTED_EDGE ( 'NONE', *, *, #10445, .F. ) ;
#1402 = LINE ( 'NONE', #20781, #4685 ) ;
#1403 = CARTESIAN_POINT ( 'NONE',  ( 215.1694833127197057, 20.95620526910698445, -14.00000000000008527 ) ) ;
#1404 = CARTESIAN_POINT ( 'NONE',  ( -15.99999999999999289, 80.00000000000000000, 4.999999999999989342 ) ) ;
#1405 = DIRECTION ( 'NONE',  ( -0.8660254037844357100, -0.5000000000000051070, 0.000000000000000000 ) ) ;
#1406 = AXIS2_PLACEMENT_3D ( 'NONE', #3019, #7571, #20811 ) ;
#1407 = CARTESIAN_POINT ( 'NONE',  ( 5.000000000000000000, -2.342598717236910932, -4.057499999999996554 ) ) ;
#1408 = CARTESIAN_POINT ( 'NONE',  ( 210.9308365141136790, 12.89766362403163491, -24.52223341984404570 ) ) ;
#1409 = EDGE_CURVE ( 'NONE', #2714, #10603, #16734, .T. ) ;
#1410 = VECTOR ( 'NONE', #159, 1000.000000000000114 ) ;
#1411 = LINE ( 'NONE', #20788, #14012 ) ;
#1412 = DIRECTION ( 'NONE',  ( 0.8660254037844370423, 0.5000000000000027756, -6.106226635438360972E-16 ) ) ;
#1413 = PLANE ( 'NONE',  #3313 ) ;
#1414 = ORIENTED_EDGE ( 'NONE', *, *, #5727, .F. ) ;
#1415 = VECTOR ( 'NONE', #11712, 1000.000000000000227 ) ;
#1416 = FACE_BOUND ( 'NONE', #7340, .T. ) ;
#1417 = CARTESIAN_POINT ( 'NONE',  ( 58.59049733147158889, 85.48875911470162237, -11.99710087975904216 ) ) ;
#1418 = AXIS2_PLACEMENT_3D ( 'NONE', #17347, #9265, #19043 ) ;
#1419 = DIRECTION ( 'NONE',  ( 0.000000000000000000, 0.000000000000000000, -1.000000000000000000 ) ) ;
#1420 = CARTESIAN_POINT ( 'NONE',  ( -28.48686108716033516, 80.00000000007401013, -0.6469719004584603139 ) ) ;
#1422 = ORIENTED_EDGE ( 'NONE', *, *, #8317, .T. ) ;
#1421 = VERTEX_POINT ( 'NONE', #14005 ) ;
#1423 = EDGE_LOOP ( 'NONE', ( #15729, #19961, #20861, #4129, #20202, #13171, #20531 ) ) ;
#1424 = CARTESIAN_POINT ( 'NONE',  ( 229.3257029665984419, 37.51163360410157566, -16.29291827778590118 ) ) ;
#1425 = PRESENTATION_LAYER_ASSIGNMENT (  '', '', ( #6820 ) ) ;
#1426 = CARTESIAN_POINT ( 'NONE',  ( 222.0051070464462271, 32.11665437128451828, -14.55011169161702078 ) ) ;
#1427 = ORIENTED_EDGE ( 'NONE', *, *, #2150, .T. ) ;
#1428 = CARTESIAN_POINT ( 'NONE',  ( 220.0479314030272064, 35.09471172164835906, -17.56803216753791475 ) ) ;
#1429 = CARTESIAN_POINT ( 'NONE',  ( -27.61765422622016430, 80.00000000021789504, -4.628091497302904145 ) ) ;
#1430 = VECTOR ( 'NONE', #5416, 1000.000000000000227 ) ;
#1431 = DIRECTION ( 'NONE',  ( 0.8660254037844375974, 0.5000000000000019984, 4.163336342344337520E-16 ) ) ;
#1432 = B_SPLINE_CURVE_WITH_KNOTS ( 'NONE', 3,
 ( #9831, #19482, #11027, #4963 ),
 .UNSPECIFIED., .F., .F.,
 ( 4, 4 ),
 ( 4.336808689942017736E-18, 0.001415162808320489293 ),
 .UNSPECIFIED. ) ;
#1433 = VERTEX_POINT ( 'NONE', #20449 ) ;
#1434 = CARTESIAN_POINT ( 'NONE',  ( 188.9132435853528591, 28.89116896218934016, -16.92893218813457068 ) ) ;
#1435 = ORIENTED_EDGE ( 'NONE', *, *, #6398, .T. ) ;
#1436 = FACE_OUTER_BOUND ( 'NONE', #3782, .T. ) ;
#1437 = CARTESIAN_POINT ( 'NONE',  ( 5.000000000000000000, 2.342598717236900718, -4.057500000000001883 ) ) ;
#1438 = LINE ( 'NONE', #16173, #5723 ) ;
#1439 = LINE ( 'NONE', #15662, #5742 ) ;
#1440 = VERTEX_POINT ( 'NONE', #10589 ) ;
#1441 = DIRECTION ( 'NONE',  ( 0.03412120668232990900, -0.05909966358935514474, 0.9976687691905399280 ) ) ;
#1442 = CIRCLE ( 'NONE', #14325, 4.400000000000000355 ) ;
#1443 = AXIS2_PLACEMENT_3D ( 'NONE', #5680, #2317, #12170 ) ;
#1444 = ORIENTED_EDGE ( 'NONE', *, *, #18603, .T. ) ;
#1445 = B_SPLINE_CURVE_WITH_KNOTS ( 'NONE', 3,
 ( #9747, #19409, #127, #9649 ),
 .UNSPECIFIED., .F., .F.,
 ( 4, 4 ),
 ( 8.181520800210985107E-07, 0.0004528713938598570360 ),
 .UNSPECIFIED. ) ;
#1446 = CARTESIAN_POINT ( 'NONE',  ( 200.0157312721003393, 23.75418783301503467, -14.00000000000005507 ) ) ;
#1447 = DIRECTION ( 'NONE',  ( 1.000000000000000000, 0.000000000000000000, 0.000000000000000000 ) ) ;
#1448 = CARTESIAN_POINT ( 'NONE',  ( 229.3566434666465170, 37.45804308600666843, -11.78314368930809231 ) ) ;
#1449 = DIRECTION ( 'NONE',  ( -0.5000000000000047740, 0.8660254037844358210, 0.000000000000000000 ) ) ;
#1450 = ADVANCED_FACE ( 'NONE', ( #16963 ), #5914, .T. ) ;
#1451 = DIRECTION ( 'NONE',  ( -0.5000000000000043299, 0.8660254037844361541, 1.272130549049658454E-16 ) ) ;
#1452 = ORIENTED_EDGE ( 'NONE', *, *, #6302, .F. ) ;
#1453 = CARTESIAN_POINT ( 'NONE',  ( 212.2669970461267042, 13.31505690926096364, -24.01557619556987788 ) ) ;
#1454 = AXIS2_PLACEMENT_3D ( 'NONE', #933, #10349, #10453 ) ;
#1455 = VERTEX_POINT ( 'NONE', #2551 ) ;
#1456 = CARTESIAN_POINT ( 'NONE',  ( 64.92628429094538944, 80.60227088397526529, -21.04771496906974448 ) ) ;
#1457 = CARTESIAN_POINT ( 'NONE',  ( -7.049456388680209074, 44.99877348914139930, -8.732428919826512370 ) ) ;
#1458 = PLANE ( 'NONE',  #17046 ) ;
#1459 = DIRECTION ( 'NONE',  ( 0.5000000000000044409, -0.8660254037844360431, -4.006172263299080068E-16 ) ) ;
#1460 = CARTESIAN_POINT ( 'NONE',  ( 98.91428619100412334, 200.0914894846854679, 13.49999999999996803 ) ) ;
#1462 = VERTEX_POINT ( 'NONE', #5816 ) ;
#1461 = VERTEX_POINT ( 'NONE', #18446 ) ;
#1463 = DIRECTION ( 'NONE',  ( 1.000000000000000000, 0.000000000000000000, 0.000000000000000000 ) ) ;
#1464 = DIRECTION ( 'NONE',  ( 0.5000000000000057732, -0.8660254037844353769, 0.000000000000000000 ) ) ;
#1465 = CARTESIAN_POINT ( 'NONE',  ( -11.00827370573233566, 79.99999999999128875, -11.47115151921867238 ) ) ;
#1466 = VERTEX_POINT ( 'NONE', #12416 ) ;
#1467 = VERTEX_POINT ( 'NONE', #18870 ) ;
#1468 = ORIENTED_EDGE ( 'NONE', *, *, #11042, .F. ) ;
#1469 = DIRECTION ( 'NONE',  ( 0.5000000000000046629, -0.8660254037844360431, 0.000000000000000000 ) ) ;
#1470 = CARTESIAN_POINT ( 'NONE',  ( 214.4667135392577961, 16.34067451675213434, -14.00000000000005507 ) ) ;
#1471 = CARTESIAN_POINT ( 'NONE',  ( 216.2725394319739110, 15.91768827161142674, -14.00000000000005507 ) ) ;
#1472 = CARTESIAN_POINT ( 'NONE',  ( 28.00000000000001066, 65.00000000000000000, -12.50000000000000000 ) ) ;
#1473 = ORIENTED_EDGE ( 'NONE', *, *, #16783, .T. ) ;
#1474 = EDGE_CURVE ( 'NONE', #10313, #10227, #2340, .T. ) ;
#1475 = VERTEX_POINT ( 'NONE', #8898 ) ;
#1476 = ADVANCED_FACE ( 'NONE', ( #8996, #20035 ), #12312, .T. ) ;
#1477 = CARTESIAN_POINT ( 'NONE',  ( 0.2373305082636106289, 69.70612202061965945, 1.777571403100949743 ) ) ;
#1478 = CARTESIAN_POINT ( 'NONE',  ( 227.9553588074475954, 39.88513931160571957, -14.00000000000005507 ) ) ;
#1479 = EDGE_CURVE ( 'NONE', #2018, #7001, #5828, .T. ) ;
#1480 = B_SPLINE_CURVE_WITH_KNOTS ( 'NONE', 3,
 ( #878, #2892, #18792, #984 ),
 .UNSPECIFIED., .F., .F.,
 ( 4, 4 ),
 ( 2.816680711908978775E-07, 0.0006729324601288649149 ),
 .UNSPECIFIED. ) ;
#1481 = CARTESIAN_POINT ( 'NONE',  ( -35.00000000000000000, 65.00000000000000000, -12.50000000000000000 ) ) ;
#1483 = CARTESIAN_POINT ( 'NONE',  ( -31.99680141974825531, 61.98207243580021242, 2.197686203131483662 ) ) ;
#1482 = ADVANCED_BREP_SHAPE_REPRESENTATION ( '', ( #10492, #18233 ), #11452 ) ;
#1484 = CARTESIAN_POINT ( 'NONE',  ( 226.6211368133091923, 39.11482588413117867, -14.00000000000005507 ) ) ;
#1485 = AXIS2_PLACEMENT_3D ( 'NONE', #4261, #10715, #2678 ) ;
#1486 = CARTESIAN_POINT ( 'NONE',  ( -27.32414976724623301, 67.00845937186198853, 5.293280639215754313 ) ) ;
#1487 = CARTESIAN_POINT ( 'NONE',  ( -34.00000000000000711, 65.00000000000000000, -12.50000000000000000 ) ) ;
#1488 = CARTESIAN_POINT ( 'NONE',  ( 27.00000000000002487, 64.25000000000000000, 2.481238266578627449 ) ) ;
#1489 = ORIENTED_EDGE ( 'NONE', *, *, #12667, .F. ) ;
#1491 = ADVANCED_FACE ( 'NONE', ( #7399 ), #9603, .T. ) ;
#1490 = CARTESIAN_POINT ( 'NONE',  ( 82.46725602463313010, 64.79916592910645079, 0.6251661754290179784 ) ) ;
#1492 = VERTEX_POINT ( 'NONE', #20548 ) ;
#1493 = ORIENTED_EDGE ( 'NONE', *, *, #2131, .F. ) ;
#1494 = CARTESIAN_POINT ( 'NONE',  ( -3.243958593759534104, 64.25000000000001421, 3.524958307384021161 ) ) ;
#1495 = CARTESIAN_POINT ( 'NONE',  ( 209.3577481411912231, 3.480248335904264856, -14.00000000000005507 ) ) ;
#1496 = ADVANCED_FACE ( 'NONE', ( #13106 ), #11502, .F. ) ;
#1497 = DIRECTION ( 'NONE',  ( -0.5000000000000029976, 0.8660254037844370423, 0.000000000000000000 ) ) ;
#1498 = ORIENTED_EDGE ( 'NONE', *, *, #7269, .T. ) ;
#1499 = SHAPE_DEFINITION_REPRESENTATION ( #14006, #8398 ) ;
#1500 = DIRECTION ( 'NONE',  ( -0.5000000000000025535, 0.8660254037844372643, 0.000000000000000000 ) ) ;
#1501 = ORIENTED_EDGE ( 'NONE', *, *, #18459, .F. ) ;
#1502 = CARTESIAN_POINT ( 'NONE',  ( 194.1867014016589508, 7.531440531094472313, -18.06789442459577444 ) ) ;
#1503 = CARTESIAN_POINT ( 'NONE',  ( 86.00000000000000000, 65.00000000000000000, -12.50000000000000000 ) ) ;
#1504 = CARTESIAN_POINT ( 'NONE',  ( 210.0699630922315748, 29.36925333534437499, -16.49993777872327527 ) ) ;
#1505 = CARTESIAN_POINT ( 'NONE',  ( 4.000000000000000000, 3.518949890710767026, -4.987329993433320396E-15 ) ) ;
#1506 = ADVANCED_FACE ( 'NONE', ( #17384 ), #8308, .F. ) ;
#1507 = EDGE_CURVE ( 'NONE', #7814, #1900, #6505, .T. ) ;
#1508 = DIRECTION ( 'NONE',  ( -0.5000000000000049960, 0.8660254037844357100, -0.000000000000000000 ) ) ;
#1509 = DIRECTION ( 'NONE',  ( -0.000000000000000000, -1.000000000000000000, -0.000000000000000000 ) ) ;
#1510 = PLANE ( 'NONE',  #13226 ) ;
#1511 = LINE ( 'NONE', #3303, #4175 ) ;
#1512 = DIRECTION ( 'NONE',  ( -0.8660254037844361541, -0.5000000000000045519, 8.850264995343375625E-15 ) ) ;
#1513 = CARTESIAN_POINT ( 'NONE',  ( 202.6305150283801026, 8.282480684066333865, -25.48492467622465441 ) ) ;
#1514 = EDGE_LOOP ( 'NONE', ( #7636, #5356, #53, #5961 ) ) ;
#1515 = VECTOR ( 'NONE', #12672, 999.9999999999998863 ) ;
#1517 = EDGE_CURVE ( 'NONE', #1689, #7288, #16483, .T. ) ;
#1516 = DIRECTION ( 'NONE',  ( 0.000000000000000000, -0.9982500481053675490, 0.05913409725049680044 ) ) ;
#1518 = CARTESIAN_POINT ( 'NONE',  ( 82.69314351557979137, 60.01919287894784105, -0.1021492064584022391 ) ) ;
#1519 = CARTESIAN_POINT ( 'NONE',  ( 182.3972143829816446, 2.035126980567696364, -22.00000000000003908 ) ) ;
#1520 = CARTESIAN_POINT ( 'NONE',  ( 44.99529059433372424, 246.0222400402097946, -8.999999999999973355 ) ) ;
#1522 = VERTEX_POINT ( 'NONE', #20650 ) ;
#1521 = VERTEX_POINT ( 'NONE', #13209 ) ;
#1523 = VERTEX_POINT ( 'NONE', #1862 ) ;
#1524 = ORIENTED_EDGE ( 'NONE', *, *, #171, .T. ) ;
#1525 = FILL_AREA_STYLE_COLOUR ( '', #20042 ) ;
#1526 = EDGE_CURVE ( 'NONE', #19313, #2754, #9894, .T. ) ;
#1527 = ORIENTED_EDGE ( 'NONE', *, *, #14882, .F. ) ;
#1528 = B_SPLINE_CURVE_WITH_KNOTS ( 'NONE', 3,
 ( #2709, #15652, #1120, #7563 ),
 .UNSPECIFIED., .F., .F.,
 ( 4, 4 ),
 ( 0.000000000000000000, 0.001415162808320496448 ),
 .UNSPECIFIED. ) ;
#1529 = FACE_BOUND ( 'NONE', #1543, .T. ) ;
#1530 = EDGE_LOOP ( 'NONE', ( #1123, #6318, #16160, #7476, #6971, #5330, #6903, #19698 ) ) ;
#1531 = FACE_OUTER_BOUND ( 'NONE', #2598, .T. ) ;
#1532 = CARTESIAN_POINT ( 'NONE',  ( 215.7705878007389515, 15.51487865500265073, -18.20503500338685399 ) ) ;
#1533 = EDGE_CURVE ( 'NONE', #10626, #2349, #13431, .T. ) ;
#1534 = EDGE_LOOP ( 'NONE', ( #11958, #14108, #9602, #5050 ) ) ;
#1535 = ADVANCED_FACE ( 'NONE', ( #4449 ), #9793, .F. ) ;
#1536 = PLANE ( 'NONE',  #8185 ) ;
#1537 = EDGE_CURVE ( 'NONE', #9185, #5663, #6711, .T. ) ;
#1538 = DIRECTION ( 'NONE',  ( -0.000000000000000000, -0.000000000000000000, 1.000000000000000000 ) ) ;
#1539 = DIRECTION ( 'NONE',  ( 0.000000000000000000, 0.5000000000000009992, 0.8660254037844380415 ) ) ;
#1540 = ORIENTED_EDGE ( 'NONE', *, *, #15388, .T. ) ;
#1541 = DIRECTION ( 'NONE',  ( -0.8660254037844358210, -0.5000000000000049960, 0.000000000000000000 ) ) ;
#1542 = CARTESIAN_POINT ( 'NONE',  ( 54.01452848080093361, 170.4004617752990498, 4.000000000000000000 ) ) ;
#1543 = EDGE_LOOP ( 'NONE', ( #7691, #17063 ) ) ;
#1544 = CIRCLE ( 'NONE', #20817, 13.49999999999999645 ) ;
#1545 = LINE ( 'NONE', #8086, #1740 ) ;
#1546 = ORIENTED_EDGE ( 'NONE', *, *, #18168, .T. ) ;
#1547 = AXIS2_PLACEMENT_3D ( 'NONE', #1922, #11882, #19602 ) ;
#1548 = FACE_OUTER_BOUND ( 'NONE', #20054, .T. ) ;
#1549 = FACE_OUTER_BOUND ( 'NONE', #4665, .T. ) ;
#1550 = AXIS2_PLACEMENT_3D ( 'NONE', #3099, #1508, #11566 ) ;
#1551 = CARTESIAN_POINT ( 'NONE',  ( 219.7290174349947165, 34.13358052910027141, -18.16400186620062485 ) ) ;
#1552 = CARTESIAN_POINT ( 'NONE',  ( 227.9553588074475670, 39.88513931160575510, -14.00000000000005507 ) ) ;
#1553 = CARTESIAN_POINT ( 'NONE',  ( -30.00000000000017408, 4.999999999999888090, -5.972363130614329663 ) ) ;
#1554 = ORIENTED_EDGE ( 'NONE', *, *, #5736, .T. ) ;
#1555 = CARTESIAN_POINT ( 'NONE',  ( 209.0038672028605617, 11.96213727764295598, -11.52983444460693008 ) ) ;
#1556 = ORIENTED_EDGE ( 'NONE', *, *, #17828, .F. ) ;
#1557 = AXIS2_PLACEMENT_3D ( 'NONE', #20567, #14134, #9533 ) ;
#1558 = CARTESIAN_POINT ( 'NONE',  ( -9.459184262262997578, 45.14452168132807230, -10.67415978328379644 ) ) ;
#1559 = CARTESIAN_POINT ( 'NONE',  ( 228.9601487287870043, 37.49183298441048606, -11.19450202347640122 ) ) ;
#1560 = VECTOR ( 'NONE', #12071, 1000.000000000000114 ) ;
#1561 = DIRECTION ( 'NONE',  ( 1.000000000000000000, 0.000000000000000000, 0.000000000000000000 ) ) ;
#1562 = CARTESIAN_POINT ( 'NONE',  ( 97.35757311143078141, 199.0198733241707600, 12.65155119472265710 ) ) ;
#1563 = EDGE_CURVE ( 'NONE', #1231, #20270, #14115, .T. ) ;
#1564 = ORIENTED_EDGE ( 'NONE', *, *, #13958, .F. ) ;
#1565 = ORIENTED_EDGE ( 'NONE', *, *, #4070, .T. ) ;
#1566 = CARTESIAN_POINT ( 'NONE',  ( 218.4545804407782157, 37.82445173649187353, -15.97403403822083767 ) ) ;
#1567 = CARTESIAN_POINT ( 'NONE',  ( 194.1738290307969805, 7.524008664312185957, -9.972943347741734854 ) ) ;
#1568 = CARTESIAN_POINT ( 'NONE',  ( -11.91377925401460303, 79.99311222855632764, -11.99929078098838353 ) ) ;
#1569 = ORIENTED_EDGE ( 'NONE', *, *, #8317, .F. ) ;
#1570 = ORIENTED_EDGE ( 'NONE', *, *, #10314, .T. ) ;
#1571 = ORIENTED_EDGE ( 'NONE', *, *, #12337, .T. ) ;
#1572 = LINE ( 'NONE', #4849, #18010 ) ;
#1573 = CARTESIAN_POINT ( 'NONE',  ( 5.000000000000004441, 0.000000000000000000, 0.000000000000000000 ) ) ;
#1574 = CARTESIAN_POINT ( 'NONE',  ( -31.96031196521626683, 62.29327126685349469, 2.258945850240144271 ) ) ;
#1575 = CONICAL_SURFACE ( 'NONE', #10354, 4.171999999999999709, 0.7853981633974687071 ) ;
#1576 = CARTESIAN_POINT ( 'NONE',  ( -12.97569482790883910, 59.73889726494167007, -3.991204510516653148 ) ) ;
#1577 = ORIENTED_EDGE ( 'NONE', *, *, #12902, .F. ) ;
#1578 = ORIENTED_EDGE ( 'NONE', *, *, #7221, .F. ) ;
#1579 = CIRCLE ( 'NONE', #13424, 15.00000000000001954 ) ;
#1580 = LINE ( 'NONE', #6016, #13806 ) ;
#1581 = VECTOR ( 'NONE', #10544, 1000.000000000000000 ) ;
#1582 = EDGE_CURVE ( 'NONE', #4169, #5897, #12618, .T. ) ;
#1583 = DIRECTION ( 'NONE',  ( -0.5943026915289566503, -0.3431208189343668002, 0.7273736415730551741 ) ) ;
#1584 = DIRECTION ( 'NONE',  ( -0.8137976813493681405, -0.4698463103929584328, 0.3420201433256762624 ) ) ;
#1585 = CARTESIAN_POINT ( 'NONE',  ( -32.44758470016270024, 59.24237906757368677, 1.369529638433351737 ) ) ;
#1586 = CARTESIAN_POINT ( 'NONE',  ( 68.05653244943854929, 72.05492144323341108, -23.45593384645862045 ) ) ;
#1587 = EDGE_CURVE ( 'NONE', #11760, #1337, #2864, .T. ) ;
#1588 = VERTEX_POINT ( 'NONE', #19080 ) ;
#1589 = CARTESIAN_POINT ( 'NONE',  ( 208.4761278624580711, 5.007259451653140125, -14.00000000000005507 ) ) ;
#1590 = DIRECTION ( 'NONE',  ( -1.000000000000000000, -0.000000000000000000, -0.000000000000000000 ) ) ;
#1591 = PLANE ( 'NONE',  #12909 ) ;
#1592 = AXIS2_PLACEMENT_3D ( 'NONE', #582, #684, #8524 ) ;
#1593 = EDGE_CURVE ( 'NONE', #255, #1746, #12510, .T. ) ;
#1594 = VERTEX_POINT ( 'NONE', #18972 ) ;
#1595 = CARTESIAN_POINT ( 'NONE',  ( 60.86250686525652753, 83.74154639049930893, -7.143441593098562414 ) ) ;
#1596 = ORIENTED_EDGE ( 'NONE', *, *, #9727, .F. ) ;
#1597 = VERTEX_POINT ( 'NONE', #8204 ) ;
#1598 = CARTESIAN_POINT ( 'NONE',  ( -4.615602823079929529, 68.36083330499455712, 5.162430512331780186 ) ) ;
#1599 = CARTESIAN_POINT ( 'NONE',  ( 208.4761278624580711, 5.007259451653140125, -14.00000000000005507 ) ) ;
#1600 = ORIENTED_EDGE ( 'NONE', *, *, #16947, .T. ) ;
#1601 = CARTESIAN_POINT ( 'NONE',  ( -28.42834865230874541, 79.61890673690945164, -9.096465090019584920 ) ) ;
#1602 = B_SPLINE_CURVE_WITH_KNOTS ( 'NONE', 3,
 ( #20100, #5665, #7055, #10225 ),
 .UNSPECIFIED., .F., .F.,
 ( 4, 4 ),
 ( 0.0005365470222895969915, 0.0005856888230752368800 ),
 .UNSPECIFIED. ) ;
#1603 = DIRECTION ( 'NONE',  ( -1.000000000000000000, 0.000000000000000000, 0.000000000000000000 ) ) ;
#1604 = ORIENTED_EDGE ( 'NONE', *, *, #6782, .T. ) ;
#1605 = AXIS2_PLACEMENT_3D ( 'NONE', #3807, #5810, #8684 ) ;
#1606 = DIRECTION ( 'NONE',  ( -0.8089634933040120712, 0.000000000000000000, 0.5878588831525550784 ) ) ;
#1607 = CARTESIAN_POINT ( 'NONE',  ( 209.1488401613018198, 31.20282942076142518, -15.65137675853565646 ) ) ;
#1608 = FACE_OUTER_BOUND ( 'NONE', #671, .T. ) ;
#1609 = AXIS2_PLACEMENT_3D ( 'NONE', #14330, #6537, #20762 ) ;
#1610 = CARTESIAN_POINT ( 'NONE',  ( 32.36389338619004263, 157.9004617752989930, -12.50000000000000000 ) ) ;
#1611 = CARTESIAN_POINT ( 'NONE',  ( 4.000000000000000000, 2.639212418033074048, -1.523750000000002602 ) ) ;
#1612 = EDGE_CURVE ( 'NONE', #14622, #14657, #4551, .T. ) ;
#1613 = CARTESIAN_POINT ( 'NONE',  ( 30.00000000000000355, 5.000000000000000000, -30.00000000000000000 ) ) ;
#1614 = CARTESIAN_POINT ( 'NONE',  ( 5.000000000000004441, 7.027796151710827388, -4.057500000000009877 ) ) ;
#1615 = DIRECTION ( 'NONE',  ( 0.8660254037844371533, 0.5000000000000025535, -6.106226635438359986E-16 ) ) ;
#1616 = EDGE_CURVE ( 'NONE', #1291, #10896, #11018, .T. ) ;
#1617 = ORIENTED_EDGE ( 'NONE', *, *, #16795, .T. ) ;
#1618 = DIRECTION ( 'NONE',  ( -0.5000000000000047740, 0.8660254037844358210, 0.000000000000000000 ) ) ;
#1619 = CARTESIAN_POINT ( 'NONE',  ( 202.7058429191241089, 0.9029637956749735350, -4.494676796018656439 ) ) ;
#1620 = AXIS2_PLACEMENT_3D ( 'NONE', #6687, #17645, #13184 ) ;
#1621 = DIRECTION ( 'NONE',  ( 0.8660254037844361541, 0.5000000000000044409, 0.000000000000000000 ) ) ;
#1622 = DIRECTION ( 'NONE',  ( 0.000000000000000000, -0.9929900419787550669, 0.1181980394551037233 ) ) ;
#1623 = VECTOR ( 'NONE', #954, 1000.000000000000000 ) ;
#1625 = ORIENTED_EDGE ( 'NONE', *, *, #82, .F. ) ;
#1624 = ORIENTED_EDGE ( 'NONE', *, *, #6295, .F. ) ;
#1626 = EDGE_CURVE ( 'NONE', #2667, #15611, #12431, .T. ) ;
#1627 = CARTESIAN_POINT ( 'NONE',  ( -31.82323003959540486, 65.74999999999997158, 2.481238266578629226 ) ) ;
#1628 = ORIENTED_EDGE ( 'NONE', *, *, #10951, .T. ) ;
#1629 = LINE ( 'NONE', #14581, #3324 ) ;
#1630 = CARTESIAN_POINT ( 'NONE',  ( -28.40027614393203237, 79.99999999992436983, -1.584264587336083219 ) ) ;
#1631 = CARTESIAN_POINT ( 'NONE',  ( 220.3053218761288861, 33.13539195642835011, -16.94731950718130875 ) ) ;
#1632 = EDGE_CURVE ( 'NONE', #3202, #8339, #7249, .T. ) ;
#1633 = ORIENTED_EDGE ( 'NONE', *, *, #16546, .T. ) ;
#1634 = CIRCLE ( 'NONE', #17557, 12.47473710546057823 ) ;
#1635 = FACE_OUTER_BOUND ( 'NONE', #16500, .T. ) ;
#1636 = ADVANCED_FACE ( 'NONE', ( #797 ), #11820, .F. ) ;
#1637 = VECTOR ( 'NONE', #20069, 999.9999999999998863 ) ;
#1638 = CARTESIAN_POINT ( 'NONE',  ( 79.60954748500523692, 66.31227659742221192, 0.4370474645863004493 ) ) ;
#1639 = LINE ( 'NONE', #12681, #3977 ) ;
#1640 = ORIENTED_EDGE ( 'NONE', *, *, #10833, .T. ) ;
#1641 = DIRECTION ( 'NONE',  ( 0.5000000000000044409, -0.8660254037844360431, -0.000000000000000000 ) ) ;
#1642 = CARTESIAN_POINT ( 'NONE',  ( 188.9132435853528591, 28.89116896218934016, -11.07106781186553768 ) ) ;
#1643 = ORIENTED_EDGE ( 'NONE', *, *, #12632, .T. ) ;
#1644 = CARTESIAN_POINT ( 'NONE',  ( 207.8564944041415004, 11.29970128344163882, -16.00578157674290125 ) ) ;
#1645 = EDGE_CURVE ( 'NONE', #16948, #3078, #11718, .T. ) ;
#1646 = ORIENTED_EDGE ( 'NONE', *, *, #7199, .T. ) ;
#1647 = EDGE_CURVE ( 'NONE', #12707, #2199, #5884, .T. ) ;
#1648 = VECTOR ( 'NONE', #9225, 1000.000000000000000 ) ;
#1649 = CARTESIAN_POINT ( 'NONE',  ( 210.8166463470705310, 28.23117696587115333, -12.01093917984183790 ) ) ;
#1650 = DIRECTION ( 'NONE',  ( -0.5000000000000029976, 0.8660254037844370423, 0.000000000000000000 ) ) ;
#1651 = CARTESIAN_POINT ( 'NONE',  ( 57.02433875312727452, 129.1873174624876413, 41.00000000000001421 ) ) ;
#1652 = CARTESIAN_POINT ( 'NONE',  ( 209.6384834804775608, 12.32853315635724556, -3.125199447383530060 ) ) ;
#1653 = CARTESIAN_POINT ( 'NONE',  ( -28.14076360089397610, 6.485357845765030937, -3.101869372784200163 ) ) ;
#1654 = CARTESIAN_POINT ( 'NONE',  ( 44.05523633727993627, 164.6504617752990498, -12.50000000000000000 ) ) ;
#1655 = EDGE_CURVE ( 'NONE', #9209, #8656, #18501, .T. ) ;
#1656 = VERTEX_POINT ( 'NONE', #3646 ) ;
#1657 = CARTESIAN_POINT ( 'NONE',  ( 75.15087072258846490, 70.53326157795075346, -24.36499220651786146 ) ) ;
#1658 = CARTESIAN_POINT ( 'NONE',  ( 201.7852296553354563, 11.91845286379962943, -1.053683606938436323 ) ) ;
#1659 = CIRCLE ( 'NONE', #19280, 9.999999999999994671 ) ;
#1660 = ORIENTED_EDGE ( 'NONE', *, *, #12462, .F. ) ;
#1661 = CARTESIAN_POINT ( 'NONE',  ( 105.7973891242897650, 30.70991617951901276, -12.50000000000000000 ) ) ;
#1662 = CARTESIAN_POINT ( 'NONE',  ( -10.67320097367628051, 45.27968546322713195, -11.31348108637220484 ) ) ;
#1663 = DIRECTION ( 'NONE',  ( -0.000000000000000000, 0.000000000000000000, 1.000000000000000000 ) ) ;
#1664 = EDGE_CURVE ( 'NONE', #18303, #11033, #10531, .T. ) ;
#1665 = EDGE_LOOP ( 'NONE', ( #4573, #10008, #7630, #18803, #535 ) ) ;
#1666 = CARTESIAN_POINT ( 'NONE',  ( 73.36131599811851345, 198.8908428320658288, 11.00000000000001066 ) ) ;
#1667 = CARTESIAN_POINT ( 'NONE',  ( 98.62918417965860840, 199.9227537566937940, 13.48335911653028596 ) ) ;
#1669 = ORIENTED_EDGE ( 'NONE', *, *, #20521, .T. ) ;
#1668 = ORIENTED_EDGE ( 'NONE', *, *, #868, .T. ) ;
#1670 = ORIENTED_EDGE ( 'NONE', *, *, #2537, .T. ) ;
#1671 = CARTESIAN_POINT ( 'NONE',  ( 204.3734207737316808, 2.380946557804465957, -25.29453042277885544 ) ) ;
#1672 = DIRECTION ( 'NONE',  ( -0.1503837331804444566, -0.08682408883347132733, -0.9848077530122061329 ) ) ;
#1673 = CARTESIAN_POINT ( 'NONE',  ( -1.754678344426114700, 79.23832348577455775, -7.772177369786309242 ) ) ;
#1674 = EDGE_LOOP ( 'NONE', ( #3864, #19996, #508, #20023 ) ) ;
#1675 = DIRECTION ( 'NONE',  ( 0.000000000000000000, 0.000000000000000000, -1.000000000000000000 ) ) ;
#1676 = DIRECTION ( 'NONE',  ( 0.5000000000000051070, -0.8660254037844358210, 0.000000000000000000 ) ) ;
#1677 = CARTESIAN_POINT ( 'NONE',  ( -32.65293543921481501, 58.27329718154535954, 0.9126919759745467653 ) ) ;
#1678 = FACE_OUTER_BOUND ( 'NONE', #15463, .T. ) ;
#1679 = ORIENTED_EDGE ( 'NONE', *, *, #12719, .T. ) ;
#1680 = AXIS2_PLACEMENT_3D ( 'NONE', #12486, #10879, #4627 ) ;
#1681 = ORIENTED_EDGE ( 'NONE', *, *, #3937, .T. ) ;
#1682 = CARTESIAN_POINT ( 'NONE',  ( 221.1128743828189158, 31.73666998506163850, -16.20791459969598591 ) ) ;
#1683 = B_SPLINE_CURVE_WITH_KNOTS ( 'NONE', 3,
 ( #17164, #2957, #9089, #17266 ),
 .UNSPECIFIED., .F., .F.,
 ( 4, 4 ),
 ( 4.524091638411281897E-05, 0.0006111671386643617023 ),
 .UNSPECIFIED. ) ;
#1684 = LINE ( 'NONE', #15905, #8770 ) ;
#1685 = B_SPLINE_CURVE_WITH_KNOTS ( 'NONE', 3,
 ( #10004, #18194, #3658, #10111 ),
 .UNSPECIFIED., .F., .F.,
 ( 4, 4 ),
 ( 5.762863496319040269E-05, 0.0009116143729456499924 ),
 .UNSPECIFIED. ) ;
#1686 = LINE ( 'NONE', #1897, #14993 ) ;
#1687 = CARTESIAN_POINT ( 'NONE',  ( -28.78142635522318926, 60.56397566246508291, 1.839220826256013464 ) ) ;
#1688 = CARTESIAN_POINT ( 'NONE',  ( -20.95922626054125004, 15.75780479222803265, 11.47416194257517041 ) ) ;
#1689 = VERTEX_POINT ( 'NONE', #16588 ) ;
#1690 = DIRECTION ( 'NONE',  ( -0.2883401610574307661, 0.4994198088140612835, -0.8169698930104472012 ) ) ;
#1691 = CARTESIAN_POINT ( 'NONE',  ( 184.9952905943350743, 3.535126980567779409, -29.00000000000008882 ) ) ;
#1692 = EDGE_LOOP ( 'NONE', ( #15892, #9863, #17810, #13286, #4435, #5929 ) ) ;
#1693 = AXIS2_PLACEMENT_3D ( 'NONE', #6289, #4611, #1332 ) ;
#1694 = CARTESIAN_POINT ( 'NONE',  ( 55.27961512323265225, 77.56072257029609318, -9.140361019020206257 ) ) ;
#1695 = AXIS2_PLACEMENT_3D ( 'NONE', #4115, #2115, #20215 ) ;
#1696 = ORIENTED_EDGE ( 'NONE', *, *, #17820, .T. ) ;
#1697 = DIRECTION ( 'NONE',  ( -1.000000000000000000, 0.000000000000000000, 2.645739781067712995E-16 ) ) ;
#1698 = CARTESIAN_POINT ( 'NONE',  ( 226.2863802629166230, 42.77589494747574861, -12.60011953066305246 ) ) ;
#1699 = ORIENTED_EDGE ( 'NONE', *, *, #3301, .F. ) ;
#1700 = CARTESIAN_POINT ( 'NONE',  ( 228.5397721961435593, 38.87290562976085795, -17.42570676230502968 ) ) ;
#1701 = CARTESIAN_POINT ( 'NONE',  ( 208.8107687779841228, 4.427644383670616079, -14.00000000000005507 ) ) ;
#1702 = ORIENTED_EDGE ( 'NONE', *, *, #12220, .F. ) ;
#1703 = EDGE_CURVE ( 'NONE', #6947, #8218, #6833, .T. ) ;
#1704 = MECHANICAL_DESIGN_GEOMETRIC_PRESENTATION_REPRESENTATION (  '', ( #5407 ), #9480 ) ;
#1705 = CARTESIAN_POINT ( 'NONE',  ( 218.7128531318510625, 38.02498348875093370, -16.48323849494058635 ) ) ;
#1706 = CARTESIAN_POINT ( 'NONE',  ( 31.00000000000000711, 65.00000000000000000, -12.50000000000000000 ) ) ;
#1707 = DIRECTION ( 'NONE',  ( 0.5000000000000049960, -0.8660254037844358210, 0.000000000000000000 ) ) ;
#1708 = AXIS2_PLACEMENT_3D ( 'NONE', #1229, #4300, #7575 ) ;
#1709 = LINE ( 'NONE', #12961, #11365 ) ;
#1710 = CARTESIAN_POINT ( 'NONE',  ( 214.1110484215691656, 14.37972046727219144, -5.993340328401894013 ) ) ;
#1711 = AXIS2_PLACEMENT_3D ( 'NONE', #5832, #12327, #4257 ) ;
#1712 = LINE ( 'NONE', #8374, #13909 ) ;
#1713 = CARTESIAN_POINT ( 'NONE',  ( 227.5312376355471145, 39.64027283883993391, -14.00000000000005507 ) ) ;
#1714 = CARTESIAN_POINT ( 'NONE',  ( 207.0274154277438754, 3.398024846849156511, -2.233628351993186101 ) ) ;
#1715 = ORIENTED_EDGE ( 'NONE', *, *, #13794, .T. ) ;
#1716 = ORIENTED_EDGE ( 'NONE', *, *, #369, .F. ) ;
#1717 = LINE ( 'NONE', #16241, #12214 ) ;
#1718 = CIRCLE ( 'NONE', #9476, 15.00000000000000000 ) ;
#1719 = CARTESIAN_POINT ( 'NONE',  ( 82.78189083499628964, 60.49709294355461253, 0.02860270449327129150 ) ) ;
#1720 = EDGE_CURVE ( 'NONE', #15392, #20411, #15740, .T. ) ;
#1721 = AXIS2_PLACEMENT_3D ( 'NONE', #3296, #17517, #9746 ) ;
#1722 = ORIENTED_EDGE ( 'NONE', *, *, #9784, .F. ) ;
#1723 = CARTESIAN_POINT ( 'NONE',  ( -15.63739925482664539, 71.60309586965422568, -4.990008254056941261 ) ) ;
#1724 = VECTOR ( 'NONE', #9757, 1000.000000000000000 ) ;
#1725 = CARTESIAN_POINT ( 'NONE',  ( 77.91922477836661187, 52.00401066416952034, -13.06454345700202424 ) ) ;
#1727 = ORIENTED_EDGE ( 'NONE', *, *, #6581, .T. ) ;
#1726 = ORIENTED_EDGE ( 'NONE', *, *, #5090, .F. ) ;
#1728 = VECTOR ( 'NONE', #1778, 1000.000000000000227 ) ;
#1729 = DIRECTION ( 'NONE',  ( -1.000000000000000000, 0.000000000000000000, 0.000000000000000000 ) ) ;
#1730 = UNCERTAINTY_MEASURE_WITH_UNIT (LENGTH_MEASURE( 1.000000000000000082E-05 ), #2942, 'distance_accuracy_value', 'NONE');
#1731 = AXIS2_PLACEMENT_3D ( 'NONE', #16410, #12923, #9813 ) ;
#1732 = EDGE_CURVE ( 'NONE', #16063, #3717, #2384, .T. ) ;
#1733 = DIRECTION ( 'NONE',  ( 0.1503837331804316890, 0.08682408883346424966, -0.9848077530122086864 ) ) ;
#1734 = ADVANCED_FACE ( 'NONE', ( #7037 ), #2076, .T. ) ;
#1735 = CARTESIAN_POINT ( 'NONE',  ( 0.3999999999999975797, 7.470345474798854293E-16, -6.099999999999999645 ) ) ;
#1736 = ORIENTED_EDGE ( 'NONE', *, *, #7040, .F. ) ;
#1737 = AXIS2_PLACEMENT_3D ( 'NONE', #6501, #8089, #4719 ) ;
#1738 = DIRECTION ( 'NONE',  ( -3.965082230804136925E-15, -7.930164461608273850E-15, 1.000000000000000000 ) ) ;
#1739 = VECTOR ( 'NONE', #13110, 1000.000000000000114 ) ;
#1740 = VECTOR ( 'NONE', #11292, 1000.000000000000227 ) ;
#1741 = EDGE_CURVE ( 'NONE', #17881, #8280, #5547, .T. ) ;
#1742 = CARTESIAN_POINT ( 'NONE',  ( 57.02843452872113517, 76.81644352065700332, -7.029764943285477408 ) ) ;
#1743 = CARTESIAN_POINT ( 'NONE',  ( -29.34689839943911238, 64.25000000000000000, 3.131020379152387623 ) ) ;
#1744 = VERTEX_POINT ( 'NONE', #5228 ) ;
#1745 = DIRECTION ( 'NONE',  ( -0.1017280065263165834, 0.1761980758562760596, -0.9790840876823235783 ) ) ;
#1746 = VERTEX_POINT ( 'NONE', #2182 ) ;
#1747 = CYLINDRICAL_SURFACE ( 'NONE', #20698, 15.00000000000000000 ) ;
#1748 = B_SPLINE_CURVE_WITH_KNOTS ( 'NONE', 3,
 ( #1921, #3918, #537, #11881 ),
 .UNSPECIFIED., .F., .F.,
 ( 4, 4 ),
 ( 4.014844339291498858E-06, 0.0004560680861191423194 ),
 .UNSPECIFIED. ) ;
#1749 = ADVANCED_FACE ( 'NONE', ( #8633 ), #15030, .F. ) ;
#1750 = VECTOR ( 'NONE', #9141, 1000.000000000000114 ) ;
#1751 = ORIENTED_EDGE ( 'NONE', *, *, #4381, .F. ) ;
#1752 = CARTESIAN_POINT ( 'NONE',  ( 211.3365836822136430, 27.55273924158569798, -13.19013634410915969 ) ) ;
#1753 = CARTESIAN_POINT ( 'NONE',  ( 218.4336835101095460, 38.50851945753705508, -15.57898118447794822 ) ) ;
#1754 = LINE ( 'NONE', #17765, #19190 ) ;
#1755 = EDGE_CURVE ( 'NONE', #8267, #8276, #2281, .T. ) ;
#1756 = AXIS2_PLACEMENT_3D ( 'NONE', #539, #642, #6989 ) ;
#1757 = CARTESIAN_POINT ( 'NONE',  ( 34.99529059433364608, 263.3427481158985302, -28.99999999999997513 ) ) ;
#1758 = DIRECTION ( 'NONE',  ( 0.000000000000000000, -1.000000000000000000, 0.000000000000000000 ) ) ;
#1759 = DIRECTION ( 'NONE',  ( 0.6946590618905487124, 0.4010615963775265858, 0.5971585917027844026 ) ) ;
#1760 = VERTEX_POINT ( 'NONE', #14914 ) ;
#1761 = B_SPLINE_CURVE_WITH_KNOTS ( 'NONE', 3,
 ( #11189, #9788, #17668, #1753 ),
 .UNSPECIFIED., .F., .F.,
 ( 4, 4 ),
 ( 8.179433510411245714E-07, 0.0004528711851308791407 ),
 .UNSPECIFIED. ) ;
#1762 = CARTESIAN_POINT ( 'NONE',  ( 76.57684527313351452, 68.08025284203007743, -25.13374168853553670 ) ) ;
#1763 = CARTESIAN_POINT ( 'NONE',  ( -4.337715088898757898, 58.14881678702032985, 4.504901070458046775 ) ) ;
#1764 = ADVANCED_FACE ( 'NONE', ( #10312 ), #15343, .T. ) ;
#1765 = EDGE_CURVE ( 'NONE', #17716, #11581, #11935, .T. ) ;
#1766 = EDGE_LOOP ( 'NONE', ( #16172, #13234, #3164, #836 ) ) ;
#1767 = FACE_OUTER_BOUND ( 'NONE', #11658, .T. ) ;
#1768 = CARTESIAN_POINT ( 'NONE',  ( -3.348706032858273396, 64.03431171952128409, 2.490437087486337298 ) ) ;
#1769 = LINE ( 'NONE', #6618, #14371 ) ;
#1770 = CIRCLE ( 'NONE', #13629, 15.00000000000000000 ) ;
#1771 = CARTESIAN_POINT ( 'NONE',  ( 5.000000000000000000, 2.342598717236900718, -4.057500000000001883 ) ) ;
#1772 = PRESENTATION_LAYER_ASSIGNMENT (  '', '', ( #19045 ) ) ;
#1773 = LINE ( 'NONE', #13115, #20854 ) ;
#1775 = ORIENTED_EDGE ( 'NONE', *, *, #10252, .F. ) ;
#1774 = EDGE_LOOP ( 'NONE', ( #1414, #5592, #7610, #17747, #12350, #20491 ) ) ;
#1776 = EDGE_LOOP ( 'NONE', ( #10462, #16999, #6651, #485, #4901 ) ) ;
#1777 = ORIENTED_EDGE ( 'NONE', *, *, #10252, .T. ) ;
#1778 = DIRECTION ( 'NONE',  ( -0.5000000000000049960, 0.8660254037844358210, -0.000000000000000000 ) ) ;
#1779 = CARTESIAN_POINT ( 'NONE',  ( 28.00000000000001066, 65.00000000000000000, -12.50000000000000000 ) ) ;
#1780 = EDGE_CURVE ( 'NONE', #8339, #20025, #11662, .T. ) ;
#1781 = ORIENTED_EDGE ( 'NONE', *, *, #13560, .T. ) ;
#1782 = EDGE_LOOP ( 'NONE', ( #10897, #13519, #16878, #2698, #556, #15768, #8331 ) ) ;
#1783 = CARTESIAN_POINT ( 'NONE',  ( -19.90328892528527405, 61.49158825347216606, -3.129485610713140353 ) ) ;
#1784 = DIRECTION ( 'NONE',  ( -1.000000000000000000, 0.000000000000000000, 0.000000000000000000 ) ) ;
#1785 = CARTESIAN_POINT ( 'NONE',  ( -33.26897445441569801, 55.37895663941098690, -0.9854948372298418802 ) ) ;
#1786 = ORIENTED_EDGE ( 'NONE', *, *, #277, .T. ) ;
#1787 = EDGE_LOOP ( 'NONE', ( #547, #12497, #8991, #8020, #13831 ) ) ;
#1788 = B_SPLINE_CURVE_WITH_KNOTS ( 'NONE', 3,
 ( #17763, #3231, #11396, #7892 ),
 .UNSPECIFIED., .F., .F.,
 ( 4, 4 ),
 ( 4.692417266429781039E-07, 0.0008544549797053814250 ),
 .UNSPECIFIED. ) ;
#1789 = CARTESIAN_POINT ( 'NONE',  ( 229.0056296929136295, 38.06601677626851910, -11.10922658182128586 ) ) ;
#1790 = ADVANCED_FACE ( 'NONE', ( #18601 ), #17016, .F. ) ;
#1792 = ORIENTED_EDGE ( 'NONE', *, *, #7559, .F. ) ;
#1791 = CIRCLE ( 'NONE', #17012, 3.902363844300875240 ) ;
#1793 = CIRCLE ( 'NONE', #16349, 5.000000000000000000 ) ;
#1794 = CARTESIAN_POINT ( 'NONE',  ( 220.6916435225954842, 33.94974481904590391, -17.22762539913933821 ) ) ;
#1795 = ADVANCED_FACE ( 'NONE', ( #14057 ), #1219, .F. ) ;
#1796 = SHAPE_REPRESENTATION ( 'V-Trough Drill Bit Carrier Bed', ( #18233 ), #14188 ) ;
#1797 = DIRECTION ( 'NONE',  ( -0.5000000000000054401, 0.8660254037844354880, -0.000000000000000000 ) ) ;
#1798 = CARTESIAN_POINT ( 'NONE',  ( -27.29420858402278682, 64.79389399373982883, 5.356384271183856960 ) ) ;
#1799 = CARTESIAN_POINT ( 'NONE',  ( 222.0023333938010524, 32.32743654455861559, -15.57898118447804769 ) ) ;
#1800 = DIRECTION ( 'NONE',  ( 0.000000000000000000, -0.8660254037844395958, -0.4999999999999984457 ) ) ;
#1801 = DIRECTION ( 'NONE',  ( -0.8660254037844355990, -0.5000000000000054401, 2.642119490368404866E-15 ) ) ;
#1802 = ORIENTED_EDGE ( 'NONE', *, *, #8441, .F. ) ;
#1803 = CIRCLE ( 'NONE', #11622, 3.902363844300875240 ) ;
#1804 = CARTESIAN_POINT ( 'NONE',  ( 62.19571619003149010, 78.41436756500478111, -11.69768420993622904 ) ) ;
#1805 = ORIENTED_EDGE ( 'NONE', *, *, #20779, .T. ) ;
#1806 = CARTESIAN_POINT ( 'NONE',  ( 221.1519434606206005, 33.18250674572787062, -11.35524774226752598 ) ) ;
#1807 = DIRECTION ( 'NONE',  ( 0.1674398060854952741, -0.2900142513495578278, -0.9422609221188190665 ) ) ;
#1808 = CARTESIAN_POINT ( 'NONE',  ( 32.39721438298033007, 261.8427481158985302, -22.00000000000000355 ) ) ;
#1809 = B_SPLINE_CURVE_WITH_KNOTS ( 'NONE', 3,
 ( #6493, #19243, #4817, #3432 ),
 .UNSPECIFIED., .F., .F.,
 ( 4, 4 ),
 ( 1.346642366771964546E-06, 0.0004533998841466679343 ),
 .UNSPECIFIED. ) ;
#1810 = CARTESIAN_POINT ( 'NONE',  ( -27.50181195973150494, 65.74999999999997158, 4.917720511238727887 ) ) ;
#1811 = VERTEX_POINT ( 'NONE', #9149 ) ;
#1812 = CARTESIAN_POINT ( 'NONE',  ( 215.3534639294407782, 15.62807865697965504, -9.913166705713923221 ) ) ;
#1813 = AXIS2_PLACEMENT_3D ( 'NONE', #9999, #7543, #10724 ) ;
#1814 = CARTESIAN_POINT ( 'NONE',  ( 10.49211908931699178, -24.14213562373095456, 0.000000000000000000 ) ) ;
#1815 = ORIENTED_EDGE ( 'NONE', *, *, #13061, .T. ) ;
#1816 = CARTESIAN_POINT ( 'NONE',  ( 205.0662616026534693, 10.91332106064940888, -14.00000000000005507 ) ) ;
#1817 = LINE ( 'NONE', #20687, #12630 ) ;
#1818 = VERTEX_POINT ( 'NONE', #7669 ) ;
#1819 = DIRECTION ( 'NONE',  ( 0.8660254037844360431, 0.5000000000000044409, -5.976026924694053325E-17 ) ) ;
#1820 = DIRECTION ( 'NONE',  ( -0.5000000000000047740, 0.8660254037844358210, 0.000000000000000000 ) ) ;
#1821 = CARTESIAN_POINT ( 'NONE',  ( 0.000000000000000000, 0.000000000000000000, 0.000000000000000000 ) ) ;
#1822 = ORIENTED_EDGE ( 'NONE', *, *, #1008, .F. ) ;
#1823 = CYLINDRICAL_SURFACE ( 'NONE', #6787, 4.999999999999989342 ) ;
#1824 = CARTESIAN_POINT ( 'NONE',  ( 78.98475196968189493, 69.17512925677146995, 0.4016226566437379741 ) ) ;
#1825 = ADVANCED_FACE ( 'NONE', ( #12567 ), #9281, .T. ) ;
#1826 = ORIENTED_EDGE ( 'NONE', *, *, #13551, .F. ) ;
#1827 = DIRECTION ( 'NONE',  ( -0.8660254037844380415, -0.5000000000000014433, -0.000000000000000000 ) ) ;
#1828 = CIRCLE ( 'NONE', #18066, 1.499999999999993783 ) ;
#1829 = CARTESIAN_POINT ( 'NONE',  ( 75.20419437876392976, 52.23006250689047647, -10.01053177166429542 ) ) ;
#1830 = CIRCLE ( 'NONE', #8241, 1.000000000000000888 ) ;
#1831 = B_SPLINE_CURVE_WITH_KNOTS ( 'NONE', 3,
 ( #3340, #1858, #9789, #13205 ),
 .UNSPECIFIED., .F., .F.,
 ( 4, 4 ),
 ( 4.499189576780315060E-05, 0.0008989776337512245903 ),
 .UNSPECIFIED. ) ;
#1833 = EDGE_LOOP ( 'NONE', ( #10105, #17446, #8430, #4713 ) ) ;
#1832 = EDGE_LOOP ( 'NONE', ( #8388, #6845, #1751, #131, #19942, #18550 ) ) ;
#1834 = VERTEX_POINT ( 'NONE', #15849 ) ;
#1835 = EDGE_LOOP ( 'NONE', ( #7186, #6081, #4763, #7873, #7940 ) ) ;
#1836 = ORIENTED_EDGE ( 'NONE', *, *, #8767, .T. ) ;
#1837 = CARTESIAN_POINT ( 'NONE',  ( 228.2948337026340369, 39.29715154524894416, -10.49174204642378072 ) ) ;
#1838 = ORIENTED_EDGE ( 'NONE', *, *, #1765, .F. ) ;
#1839 = DIRECTION ( 'NONE',  ( 0.000000000000000000, -1.000000000000000000, 1.110768649713242108E-15 ) ) ;
#1840 = CARTESIAN_POINT ( 'NONE',  ( -29.39959400891148533, 77.88264414865577123, -4.670285688177608918 ) ) ;
#1841 = LINE ( 'NONE', #19841, #8681 ) ;
#1842 = CARTESIAN_POINT ( 'NONE',  ( 221.5890410698854112, 32.83730178198860727, -16.41980614534981697 ) ) ;
#1843 = VECTOR ( 'NONE', #730, 1000.000000000000227 ) ;
#1844 = EDGE_CURVE ( 'NONE', #20139, #4463, #10999, .T. ) ;
#1845 = FACE_OUTER_BOUND ( 'NONE', #1787, .T. ) ;
#1846 = AXIS2_PLACEMENT_3D ( 'NONE', #15131, #19763, #13521 ) ;
#1847 = CARTESIAN_POINT ( 'NONE',  ( 56.65135822015081146, 76.97701555849656074, -17.56718000666989354 ) ) ;
#1848 = LINE ( 'NONE', #469, #12796 ) ;
#1849 = ORIENTED_EDGE ( 'NONE', *, *, #13049, .F. ) ;
#1850 = EDGE_CURVE ( 'NONE', #20019, #13147, #15755, .T. ) ;
#1851 = DIRECTION ( 'NONE',  ( 0.000000000000000000, -6.938893903907177533E-18, -1.000000000000000000 ) ) ;
#1852 = EDGE_CURVE ( 'NONE', #11864, #8857, #6569, .T. ) ;
#1853 = VERTEX_POINT ( 'NONE', #5967 ) ;
#1854 = CARTESIAN_POINT ( 'NONE',  ( 227.1024371503596342, 41.36244295655828296, -17.19244756328590285 ) ) ;
#1855 = EDGE_LOOP ( 'NONE', ( #20664, #15592, #15356, #16604 ) ) ;
#1856 = CARTESIAN_POINT ( 'NONE',  ( -34.00000000000000711, 65.00000000000000000, -27.49999999999999645 ) ) ;
#1857 = CARTESIAN_POINT ( 'NONE',  ( 10.40000000000000568, 5.776289300541406836E-16, -5.000000000000000000 ) ) ;
#1858 = CARTESIAN_POINT ( 'NONE',  ( 216.7437086208277321, 9.265328561208580282, -21.78787861992518415 ) ) ;
#1859 = VECTOR ( 'NONE', #19529, 1000.000000000000000 ) ;
#1860 = FACE_OUTER_BOUND ( 'NONE', #8789, .T. ) ;
#1861 = CARTESIAN_POINT ( 'NONE',  ( -26.51210826115306318, 5.754273642521425813, -6.783243196509797457 ) ) ;
#1862 = CARTESIAN_POINT ( 'NONE',  ( 219.8530131173444033, 35.43232009577518227, -17.56803216753788988 ) ) ;
#1863 = ORIENTED_EDGE ( 'NONE', *, *, #11828, .F. ) ;
#1864 = PRODUCT_RELATED_PRODUCT_CATEGORY ( 'part', '', ( #17206 ) ) ;
#1865 = CARTESIAN_POINT ( 'NONE',  ( 78.39368881307802894, 68.30389099123098617, -25.10803604556682700 ) ) ;
#1866 = CARTESIAN_POINT ( 'NONE',  ( -3.498163565539533337, 49.91419972531922156, 0.4740846950075849331 ) ) ;
#1867 = ADVANCED_FACE ( 'NONE', ( #2609 ), #2815, .F. ) ;
#1868 = ORIENTED_EDGE ( 'NONE', *, *, #14937, .T. ) ;
#1869 =( NAMED_UNIT ( * ) PLANE_ANGLE_UNIT ( ) SI_UNIT ( $, .RADIAN. ) );
#1870 = CARTESIAN_POINT ( 'NONE',  ( -4.083084354063197807, 52.23701737708404380, -4.580011168034334723 ) ) ;
#1871 = DIRECTION ( 'NONE',  ( 0.000000000000000000, 0.000000000000000000, -1.000000000000000000 ) ) ;
#1872 = EDGE_CURVE ( 'NONE', #12920, #3711, #10863, .T. ) ;
#1873 = DIRECTION ( 'NONE',  ( 0.5000000000000055511, -0.8660254037844353769, 2.775557561562890735E-17 ) ) ;
#1874 = DIRECTION ( 'NONE',  ( -0.000000000000000000, -1.000000000000000000, 1.117161918529055486E-15 ) ) ;
#1875 = AXIS2_PLACEMENT_3D ( 'NONE', #4980, #8260, #18132 ) ;
#1877 = EDGE_LOOP ( 'NONE', ( #5949, #5091, #15998, #9190 ) ) ;
#1876 = EDGE_LOOP ( 'NONE', ( #7394, #14928, #19480, #9817 ) ) ;
#1878 = EDGE_LOOP ( 'NONE', ( #3906, #8354, #1025, #3153 ) ) ;
#1879 = DIRECTION ( 'NONE',  ( -0.8089634933040207310, 0.000000000000000000, -0.5878588831525431990 ) ) ;
#1880 = CARTESIAN_POINT ( 'NONE',  ( 219.6109973649995197, 35.85150367506854963, -10.49174204642374519 ) ) ;
#1881 = EDGE_CURVE ( 'NONE', #997, #17881, #20600, .T. ) ;
#1882 = VERTEX_POINT ( 'NONE', #18714 ) ;
#1883 = EDGE_LOOP ( 'NONE', ( #3229, #4307, #19456, #15845, #18900, #20146, #15930, #6724 ) ) ;
#1884 = CARTESIAN_POINT ( 'NONE',  ( -16.36260074517335283, 58.39690413034580274, -4.990008254056941261 ) ) ;
#1885 = DIRECTION ( 'NONE',  ( 0.8660254037844348218, 0.5000000000000064393, 0.000000000000000000 ) ) ;
#1886 = CARTESIAN_POINT ( 'NONE',  ( 0.000000000000000000, -2.342598717236899386, 4.057500000000001883 ) ) ;
#1887 = DIRECTION ( 'NONE',  ( -0.5000000000000045519, 0.8660254037844360431, 0.000000000000000000 ) ) ;
#1888 = ORIENTED_EDGE ( 'NONE', *, *, #15850, .F. ) ;
#1889 = EDGE_CURVE ( 'NONE', #10818, #1853, #14056, .T. ) ;
#1890 = EDGE_CURVE ( 'NONE', #14688, #627, #20713, .T. ) ;
#1891 = ORIENTED_EDGE ( 'NONE', *, *, #4582, .T. ) ;
#1892 = DIRECTION ( 'NONE',  ( 0.4999999999999995004, -0.8660254037844390407, 0.000000000000000000 ) ) ;
#1893 = VERTEX_POINT ( 'NONE', #20396 ) ;
#1894 = VECTOR ( 'NONE', #7531, 1000.000000000000227 ) ;
#1895 = CARTESIAN_POINT ( 'NONE',  ( 218.2368265400617133, 38.23163736213975028, -12.98880265512657672 ) ) ;
#1896 = ADVANCED_FACE ( 'NONE', ( #19128 ), #2497, .F. ) ;
#1897 = CARTESIAN_POINT ( 'NONE',  ( 218.0936335691685599, 36.96614847458959474, -11.35524774226742828 ) ) ;
#1898 = CARTESIAN_POINT ( 'NONE',  ( -28.34314883718211320, 47.50472042562527974, -1.997976258590732357 ) ) ;
#1899 = FACE_OUTER_BOUND ( 'NONE', #4390, .T. ) ;
#1900 = VERTEX_POINT ( 'NONE', #15444 ) ;
#1901 = EDGE_CURVE ( 'NONE', #2978, #13943, #902, .T. ) ;
#1902 = DIRECTION ( 'NONE',  ( -2.003086131649568876E-16, 3.469446951953589044E-16, -1.000000000000000000 ) ) ;
#1903 = CARTESIAN_POINT ( 'NONE',  ( 8.399999999999998579, 5.388445916248354013E-16, 4.400000000000000355 ) ) ;
#1904 = ORIENTED_EDGE ( 'NONE', *, *, #4872, .T. ) ;
#1905 = ORIENTED_EDGE ( 'NONE', *, *, #2268, .T. ) ;
#1906 = EDGE_CURVE ( 'NONE', #13379, #18096, #15079, .T. ) ;
#1907 = ADVANCED_FACE ( 'NONE', ( #4186 ), #15756, .F. ) ;
#1908 = CARTESIAN_POINT ( 'NONE',  ( 62.82311980245329153, 82.22968959821695023, -5.348578013552717003 ) ) ;
#1909 = ORIENTED_EDGE ( 'NONE', *, *, #17823, .F. ) ;
#1910 = EDGE_LOOP ( 'NONE', ( #4927, #15048, #4496, #12527, #18749 ) ) ;
#1911 = CARTESIAN_POINT ( 'NONE',  ( 210.5178922176470451, 5.670851784906956183, -2.061577111287821840 ) ) ;
#1912 = AXIS2_PLACEMENT_3D ( 'NONE', #13249, #19798, #11757 ) ;
#1913 = DIRECTION ( 'NONE',  ( 0.000000000000000000, -0.8108848540793835991, 0.5852057359806522863 ) ) ;
#1914 = EDGE_CURVE ( 'NONE', #8547, #166, #1528, .T. ) ;
#1915 = EDGE_LOOP ( 'NONE', ( #17865, #19620, #6, #15097 ) ) ;
#1916 = DIRECTION ( 'NONE',  ( 0.5000000000000054401, -0.8660254037844354880, 0.000000000000000000 ) ) ;
#1917 = EDGE_CURVE ( 'NONE', #14639, #2132, #3024, .T. ) ;
#1918 = DIRECTION ( 'NONE',  ( 0.3535533905932770060, -0.6123724356957921389, 0.7071067811865480168 ) ) ;
#1919 = ORIENTED_EDGE ( 'NONE', *, *, #12734, .T. ) ;
#1920 = VECTOR ( 'NONE', #16064, 999.9999999999998863 ) ;
#1921 = CARTESIAN_POINT ( 'NONE',  ( 218.2668715373649775, 38.79744626964149035, -13.97349461567471174 ) ) ;
#1922 = CARTESIAN_POINT ( 'NONE',  ( 43.00000000000000000, 0.000000000000000000, 0.000000000000000000 ) ) ;
#1923 = EDGE_CURVE ( 'NONE', #7969, #18781, #17221, .T. ) ;
#1924 = VECTOR ( 'NONE', #8304, 1000.000000000000227 ) ;
#1925 = FACE_OUTER_BOUND ( 'NONE', #9879, .T. ) ;
#1926 = CARTESIAN_POINT ( 'NONE',  ( 207.8872982515397609, 15.44148381043179263, -24.85758746085098991 ) ) ;
#1927 = VERTEX_POINT ( 'NONE', #14480 ) ;
#1928 = CARTESIAN_POINT ( 'NONE',  ( 89.18111854763502322, 139.4901410505960087, 41.00000000000001421 ) ) ;
#1929 = CARTESIAN_POINT ( 'NONE',  ( 67.36131599811849924, 207.2831476774790076, 11.00000000000001066 ) ) ;
#1930 = CARTESIAN_POINT ( 'NONE',  ( 215.9000602621138114, 8.778247954203701298, -22.82042918318467173 ) ) ;
#1931 = ORIENTED_EDGE ( 'NONE', *, *, #1780, .F. ) ;
#1932 = EDGE_CURVE ( 'NONE', #13637, #3499, #15956, .T. ) ;
#1933 = CARTESIAN_POINT ( 'NONE',  ( 200.4233784773551861, 6.654163220837372883, -3.334988897836806299 ) ) ;
#1934 = CARTESIAN_POINT ( 'NONE',  ( 201.8352585209308359, 26.48094985263767498, -13.60979871437957911 ) ) ;
#1935 = CARTESIAN_POINT ( 'NONE',  ( -15.99999999999999289, 0.000000000000000000, -5.999999999999989342 ) ) ;
#1936 = CARTESIAN_POINT ( 'NONE',  ( 79.67147709189563898, 50.35212617480907227, -8.215081154367272376 ) ) ;
#1938 = EDGE_LOOP ( 'NONE', ( #14408, #7446, #12643, #9895 ) ) ;
#1937 = VERTEX_POINT ( 'NONE', #11170 ) ;
#1939 = CONICAL_SURFACE ( 'NONE', #10717, 4.509097725792825528, 0.5235987755983015912 ) ;
#1940 = ORIENTED_EDGE ( 'NONE', *, *, #10019, .F. ) ;
#1941 = CARTESIAN_POINT ( 'NONE',  ( 217.1183575532814416, 31.89634291273570810, -14.00000000000004441 ) ) ;
#1942 = ORIENTED_EDGE ( 'NONE', *, *, #6092, .T. ) ;
#1943 =( NAMED_UNIT ( * ) SI_UNIT ( $, .STERADIAN. ) SOLID_ANGLE_UNIT ( ) );
#1944 = CARTESIAN_POINT ( 'NONE',  ( -21.12997896807823039, 79.99099046118983836, -11.97147087692114908 ) ) ;
#1945 = CARTESIAN_POINT ( 'NONE',  ( 80.00000000000000000, 5.298012546456577047E-16, -4.171999999999999709 ) ) ;
#1946 = LINE ( 'NONE', #16883, #6090 ) ;
#1947 = EDGE_LOOP ( 'NONE', ( #10928, #1716, #4017, #6775 ) ) ;
#1948 = EDGE_CURVE ( 'NONE', #10896, #402, #5560, .T. ) ;
#1949 = CARTESIAN_POINT ( 'NONE',  ( -35.00000000000000000, 65.74999999999997158, 2.481238266578629226 ) ) ;
#1950 = CARTESIAN_POINT ( 'NONE',  ( 71.88466637961029448, 70.33575297470315491, -0.6373663580885260416 ) ) ;
#1951 = VECTOR ( 'NONE', #13576, 1000.000000000000000 ) ;
#1952 = DIRECTION ( 'NONE',  ( 0.000000000000000000, 0.000000000000000000, -1.000000000000000000 ) ) ;
#1953 = ORIENTED_EDGE ( 'NONE', *, *, #4597, .T. ) ;
#1954 = CARTESIAN_POINT ( 'NONE',  ( 5.000000000000004441, 7.027796151710827388, -4.057500000000009877 ) ) ;
#1956 = CARTESIAN_POINT ( 'NONE',  ( 205.8264633344831225, 9.596613037118636669, -14.00000000000005507 ) ) ;
#1955 = AXIS2_PLACEMENT_3D ( 'NONE', #14799, #5313, #4911 ) ;
#1957 = DIRECTION ( 'NONE',  ( 0.000000000000000000, 6.938893903907178303E-18, 1.000000000000000000 ) ) ;
#1958 = VERTEX_POINT ( 'NONE', #20807 ) ;
#1959 = ADVANCED_FACE ( 'NONE', ( #9873 ), #3543, .T. ) ;
#1960 = CARTESIAN_POINT ( 'NONE',  ( 57.20986367771984504, 224.8659788670219939, 44.53282986889903583 ) ) ;
#1961 = DIRECTION ( 'NONE',  ( 1.000000000000000000, -0.000000000000000000, -0.000000000000000000 ) ) ;
#1962 = CARTESIAN_POINT ( 'NONE',  ( 226.6211368133091923, 39.11482588413117867, -14.00000000000005507 ) ) ;
#1963 = CARTESIAN_POINT ( 'NONE',  ( 81.73016281821475104, 56.36132269136237483, -23.36898426428367870 ) ) ;
#1964 = CARTESIAN_POINT ( 'NONE',  ( -28.22702101948337727, 8.914004613553291989, -2.683272181370100373 ) ) ;
#1965 = CARTESIAN_POINT ( 'NONE',  ( 227.8547393642149927, 40.05941729951386066, -17.61401795338996124 ) ) ;
#1966 = ORIENTED_EDGE ( 'NONE', *, *, #13190, .F. ) ;
#1967 = VECTOR ( 'NONE', #3429, 1000.000000000000227 ) ;
#1968 = EDGE_CURVE ( 'NONE', #15950, #18037, #16419, .T. ) ;
#1969 = CARTESIAN_POINT ( 'NONE',  ( 68.88680438096986336, 74.41951537632650115, -21.80366467887538917 ) ) ;
#1970 = CARTESIAN_POINT ( 'NONE',  ( -15.99999999999998934, 45.63508326896292289, -12.50000000000000000 ) ) ;
#1971 = ORIENTED_EDGE ( 'NONE', *, *, #2660, .T. ) ;
#1972 = CARTESIAN_POINT ( 'NONE',  ( 203.2093925786781767, 24.04204282662517400, -14.66612357830583946 ) ) ;
#1973 = CARTESIAN_POINT ( 'NONE',  ( 1.058706124573915330, 56.42280402523184080, -0.1889998745171357630 ) ) ;
#1974 = CARTESIAN_POINT ( 'NONE',  ( -13.67010713483751694, 79.99972648321134727, -12.39549370732874500 ) ) ;
#1975 = DIRECTION ( 'NONE',  ( 0.5000000000000044409, -0.8660254037844361541, 0.000000000000000000 ) ) ;
#1976 = FACE_OUTER_BOUND ( 'NONE', #20668, .T. ) ;
#1977 = DIRECTION ( 'NONE',  ( 0.5000000000000049960, -0.8660254037844358210, 0.000000000000000000 ) ) ;
#1978 =( GEOMETRIC_REPRESENTATION_CONTEXT ( 3 ) GLOBAL_UNCERTAINTY_ASSIGNED_CONTEXT ( ( #8067 ) ) GLOBAL_UNIT_ASSIGNED_CONTEXT ( ( #11108, #10782, #1360 ) ) REPRESENTATION_CONTEXT ( 'NONE', 'WORKASPACE' ) );
#1980 = ORIENTED_EDGE ( 'NONE', *, *, #665, .T. ) ;
#1979 = EDGE_LOOP ( 'NONE', ( #13601, #10740, #15513, #394 ) ) ;
#1981 = EDGE_LOOP ( 'NONE', ( #6855, #17925, #17018, #6878, #9837 ) ) ;
#1982 = ORIENTED_EDGE ( 'NONE', *, *, #19125, .T. ) ;
#1983 = CARTESIAN_POINT ( 'NONE',  ( -15.99999999999999289, 15.09941697557068530, 0.9999999999999991118 ) ) ;
#1984 = CARTESIAN_POINT ( 'NONE',  ( 215.8997106868019387, 9.293266993639628382, -23.06309126349817618 ) ) ;
#1985 = AXIS2_PLACEMENT_3D ( 'NONE', #5518, #869, #7005 ) ;
#1986 = EDGE_CURVE ( 'NONE', #18021, #17954, #14691, .T. ) ;
#1987 = ORIENTED_EDGE ( 'NONE', *, *, #4381, .T. ) ;
#1988 = ORIENTED_EDGE ( 'NONE', *, *, #20436, .F. ) ;
#1989 = FACE_OUTER_BOUND ( 'NONE', #12300, .T. ) ;
#1990 = LINE ( 'NONE', #16611, #4096 ) ;
#1991 = CARTESIAN_POINT ( 'NONE',  ( 213.9207374538404736, 14.44686705926026882, -6.091045511237016541 ) ) ;
#1992 = ORIENTED_EDGE ( 'NONE', *, *, #8891, .F. ) ;
#1993 = DIRECTION ( 'NONE',  ( 0.000000000000000000, 1.000000000000000000, -1.302777330458572662E-15 ) ) ;
#1994 = FACE_OUTER_BOUND ( 'NONE', #18121, .T. ) ;
#1995 = EDGE_CURVE ( 'NONE', #15941, #18395, #13922, .T. ) ;
#1996 = ORIENTED_EDGE ( 'NONE', *, *, #12220, .T. ) ;
#1997 = EDGE_CURVE ( 'NONE', #16845, #4228, #19716, .T. ) ;
#1998 = CARTESIAN_POINT ( 'NONE',  ( 216.3390813779211612, 15.84309857482137396, -12.56470246848408223 ) ) ;
#1999 = CONICAL_SURFACE ( 'NONE', #16232, 13.07248899748297433, 0.6693469023067423196 ) ;
#2000 = DIRECTION ( 'NONE',  ( -0.8660254037844354880, -0.5000000000000055511, 0.000000000000000000 ) ) ;
#2001 = CARTESIAN_POINT ( 'NONE',  ( -27.72914186237699852, 52.00221496603906246, -4.940454205004202848 ) ) ;
#2002 = CARTESIAN_POINT ( 'NONE',  ( -19.05461073270698336, 19.07106427949856808, 12.12416053983767839 ) ) ;
#2003 = PLANE ( 'NONE',  #11847 ) ;
#2004 = DIRECTION ( 'NONE',  ( -0.8660254037844380415, -0.5000000000000008882, 0.000000000000000000 ) ) ;
#2005 = ADVANCED_FACE ( 'NONE', ( #9459 ), #4907, .F. ) ;
#2006 = B_SPLINE_CURVE_WITH_KNOTS ( 'NONE', 3,
 ( #16785, #2691, #7332, #2264 ),
 .UNSPECIFIED., .F., .F.,
 ( 4, 4 ),
 ( 0.002660042459396035584, 0.003652875122883113713 ),
 .UNSPECIFIED. ) ;
#2007 = EDGE_LOOP ( 'NONE', ( #18438, #3617, #11366, #18798 ) ) ;
#2008 = CARTESIAN_POINT ( 'NONE',  ( 59.23362366115814837, 84.99461582490647515, -9.581601599933526003 ) ) ;
#2009 = EDGE_LOOP ( 'NONE', ( #17589, #3058, #9743, #1679, #9388 ) ) ;
#2010 = CIRCLE ( 'NONE', #1001, 13.50000000000000178 ) ;
#2011 = VERTEX_POINT ( 'NONE', #11382 ) ;
#2012 = ORIENTED_EDGE ( 'NONE', *, *, #2100, .T. ) ;
#2013 = CARTESIAN_POINT ( 'NONE',  ( -15.99999999999999289, -10.00000000000000000, 0.000000000000000000 ) ) ;
#2014 = DIRECTION ( 'NONE',  ( -0.8660254037844358210, -0.5000000000000049960, 0.000000000000000000 ) ) ;
#2015 = EDGE_CURVE ( 'NONE', #18575, #3590, #13384, .T. ) ;
#2016 = VERTEX_POINT ( 'NONE', #6380 ) ;
#2017 = DIRECTION ( 'NONE',  ( -0.8660254037844359321, -0.5000000000000045519, 5.976026924694053325E-17 ) ) ;
#2018 = VERTEX_POINT ( 'NONE', #19631 ) ;
#2019 = EDGE_CURVE ( 'NONE', #19831, #13880, #17857, .T. ) ;
#2020 = CARTESIAN_POINT ( 'NONE',  ( 208.8627203077920171, 26.61931772755388081, -19.61257667712965258 ) ) ;
#2021 = ORIENTED_EDGE ( 'NONE', *, *, #14700, .T. ) ;
#2022 = CARTESIAN_POINT ( 'NONE',  ( -15.99999999999999289, 80.00000000000000000, 4.999999999999989342 ) ) ;
#2023 = CARTESIAN_POINT ( 'NONE',  ( 227.2107451024802174, 40.84837900465561233, -17.51243207492514031 ) ) ;
#2024 = DIRECTION ( 'NONE',  ( 0.5000000000000044409, -0.8660254037844360431, 0.000000000000000000 ) ) ;
#2025 = CARTESIAN_POINT ( 'NONE',  ( 207.4098631234038521, 11.04183859327925354, -25.80036831778744144 ) ) ;
#2026 = B_SPLINE_CURVE_WITH_KNOTS ( 'NONE', 3,
 ( #5554, #4087, #8952, #10324 ),
 .UNSPECIFIED., .F., .F.,
 ( 4, 4 ),
 ( 2.602085213965210642E-18, 0.001415162808320503387 ),
 .UNSPECIFIED. ) ;
#2027 = EDGE_CURVE ( 'NONE', #8176, #2805, #11482, .T. ) ;
#2028 = ORIENTED_EDGE ( 'NONE', *, *, #7150, .F. ) ;
#2029 = CARTESIAN_POINT ( 'NONE',  ( 205.5965122587965084, 9.994899983462953941, -14.00000000000005507 ) ) ;
#2030 = CIRCLE ( 'NONE', #11853, 12.47473710546057823 ) ;
#2031 = CARTESIAN_POINT ( 'NONE',  ( 215.7517163971578782, 8.326610718103061970, -14.00000000000005329 ) ) ;
#2032 = CARTESIAN_POINT ( 'NONE',  ( 215.8998893078988033, 9.035756268811685032, -22.94176278698385119 ) ) ;
#2033 = EDGE_CURVE ( 'NONE', #6599, #17447, #17091, .T. ) ;
#2034 = ORIENTED_EDGE ( 'NONE', *, *, #2443, .T. ) ;
#2035 = CARTESIAN_POINT ( 'NONE',  ( 217.5085967919815175, 37.97946189697392327, -13.95097276009430587 ) ) ;
#2036 = AXIS2_PLACEMENT_3D ( 'NONE', #19418, #6677, #13173 ) ;
#2037 = LINE ( 'NONE', #6896, #17613 ) ;
#2038 = CARTESIAN_POINT ( 'NONE',  ( 78.11286510409185269, 52.36951057819560873, -9.387962703321013791 ) ) ;
#2039 = EDGE_CURVE ( 'NONE', #14614, #13770, #16165, .T. ) ;
#2041 = VERTEX_POINT ( 'NONE', #7879 ) ;
#2040 = ORIENTED_EDGE ( 'NONE', *, *, #1474, .T. ) ;
#2042 = AXIS2_PLACEMENT_3D ( 'NONE', #2483, #885, #7334 ) ;
#2043 = ORIENTED_EDGE ( 'NONE', *, *, #1582, .T. ) ;
#2044 = VECTOR ( 'NONE', #16175, 1000.000000000000227 ) ;
#2045 = DIRECTION ( 'NONE',  ( -1.000000000000000000, -0.000000000000000000, -0.000000000000000000 ) ) ;
#2046 = VERTEX_POINT ( 'NONE', #14380 ) ;
#2047 = CARTESIAN_POINT ( 'NONE',  ( 79.92771531775157712, 58.85638066918279065, -23.97260934375448471 ) ) ;
#2048 = EDGE_CURVE ( 'NONE', #11211, #14920, #505, .T. ) ;
#2049 = CARTESIAN_POINT ( 'NONE',  ( -16.26048281100938553, 80.00000000000179057, -12.49947570859690593 ) ) ;
#2050 = CARTESIAN_POINT ( 'NONE',  ( 221.7162818700265916, 32.17520342297743241, -14.17836540244689125 ) ) ;
#2051 = DIRECTION ( 'NONE',  ( 0.1674398060854861703, -0.2900142513495481134, 0.9422609221188236184 ) ) ;
#2052 = ORIENTED_EDGE ( 'NONE', *, *, #4769, .F. ) ;
#2053 = LINE ( 'NONE', #5528, #1430 ) ;
#2054 = VECTOR ( 'NONE', #4786, 1000.000000000000114 ) ;
#2055 = CARTESIAN_POINT ( 'NONE',  ( 75.36551866217324402, 68.69483139169550157, -0.02780010607275849518 ) ) ;
#2056 = LINE ( 'NONE', #19533, #7352 ) ;
#2057 = ORIENTED_EDGE ( 'NONE', *, *, #7860, .T. ) ;
#2058 = CIRCLE ( 'NONE', #1046, 12.47473710546057823 ) ;
#2059 = CARTESIAN_POINT ( 'NONE',  ( 218.1364845712607803, 10.58466899794828642, -8.415281845792092597 ) ) ;
#2060 = CARTESIAN_POINT ( 'NONE',  ( -34.00000000000000711, 65.74999999999997158, 2.481238266578629226 ) ) ;
#2061 = CIRCLE ( 'NONE', #17299, 3.047499999999999876 ) ;
#2062 = EDGE_LOOP ( 'NONE', ( #17293, #12292 ) ) ;
#2063 = CARTESIAN_POINT ( 'NONE',  ( -27.29860958162435480, 64.25000000000000000, 5.347094680480811490 ) ) ;
#2064 = CARTESIAN_POINT ( 'NONE',  ( -14.69883599711670286, 79.99994663880958967, -12.45114708389669467 ) ) ;
#2065 = VECTOR ( 'NONE', #7714, 1000.000000000000114 ) ;
#2067 = ORIENTED_EDGE ( 'NONE', *, *, #8234, .T. ) ;
#2066 = ORIENTED_EDGE ( 'NONE', *, *, #1593, .T. ) ;
#2068 = CARTESIAN_POINT ( 'NONE',  ( 208.4761278624580711, 5.007259451653140125, -14.00000000000005507 ) ) ;
#2069 = DIRECTION ( 'NONE',  ( 0.000000000000000000, 0.000000000000000000, -1.000000000000000000 ) ) ;
#2070 = CARTESIAN_POINT ( 'NONE',  ( 195.9595725116093945, 4.431010226260183593, -9.972943347741736630 ) ) ;
#2071 = VECTOR ( 'NONE', #8849, 1000.000000000000114 ) ;
#2072 = AXIS2_PLACEMENT_3D ( 'NONE', #14737, #11324, #13027 ) ;
#2073 = CARTESIAN_POINT ( 'NONE',  ( 79.61145830677504875, 68.58534652329807102, -25.47370545880939474 ) ) ;
#2074 = VECTOR ( 'NONE', #13166, 999.9999999999998863 ) ;
#2075 = CONICAL_SURFACE ( 'NONE', #16626, 11.00000000000001066, 0.7853981633974439491 ) ;
#2076 = CYLINDRICAL_SURFACE ( 'NONE', #2530, 8.000000000000000000 ) ;
#2077 = ORIENTED_EDGE ( 'NONE', *, *, #15147, .F. ) ;
#2078 = CIRCLE ( 'NONE', #13934, 0.4000000000000001887 ) ;
#2079 = CARTESIAN_POINT ( 'NONE',  ( 81.66920570542281155, 63.84695342301056797, -25.45140023156622533 ) ) ;
#2080 = CARTESIAN_POINT ( 'NONE',  ( 205.0662616026534693, 10.91332106064940888, -14.00000000000005507 ) ) ;
#2081 = EDGE_LOOP ( 'NONE', ( #19123, #6063, #19574, #13979 ) ) ;
#2082 = CARTESIAN_POINT ( 'NONE',  ( 27.33334827330880756, 64.25000000000000000, 2.147472525011946409 ) ) ;
#2083 = CARTESIAN_POINT ( 'NONE',  ( -3.106223272040122385, 58.44026525808256878, 1.004519969053611961 ) ) ;
#2084 = CARTESIAN_POINT ( 'NONE',  ( 212.8019350911804963, 7.247151567852217369, -25.29453042277899755 ) ) ;
#2085 = CARTESIAN_POINT ( 'NONE',  ( 207.4176018615383441, 11.04630655582438337, -15.90550977090996909 ) ) ;
#2086 = CARTESIAN_POINT ( 'NONE',  ( 98.36082807960120533, 199.7525165975381469, 8.580140356014970493 ) ) ;
#2087 = CIRCLE ( 'NONE', #20689, 4.730184897849355252 ) ;
#2088 = DIRECTION ( 'NONE',  ( 0.000000000000000000, 0.000000000000000000, 1.000000000000000000 ) ) ;
#2089 = B_SPLINE_CURVE_WITH_KNOTS ( 'NONE', 3,
 ( #1280, #1175, #9303, #17388 ),
 .UNSPECIFIED., .F., .F.,
 ( 4, 4 ),
 ( 5.145664763195516063E-07, 0.0005664407887728418328 ),
 .UNSPECIFIED. ) ;
#2091 = EDGE_LOOP ( 'NONE', ( #13331, #5335, #14741, #12606, #6343, #16377, #14233, #11644, #18125 ) ) ;
#2090 = EDGE_LOOP ( 'NONE', ( #12029, #17556, #1270, #16271 ) ) ;
#2092 = ORIENTED_EDGE ( 'NONE', *, *, #2963, .T. ) ;
#2093 = CARTESIAN_POINT ( 'NONE',  ( -18.48100260771138537, 10.09941697557069595, 4.999999999999990230 ) ) ;
#2095 = CARTESIAN_POINT ( 'NONE',  ( 184.9952905943349606, 3.535126980567727450, -29.00000000000001066 ) ) ;
#2094 = VECTOR ( 'NONE', #16006, 1000.000000000000227 ) ;
#2096 = CIRCLE ( 'NONE', #14645, 13.99999999999998757 ) ;
#2097 = ORIENTED_EDGE ( 'NONE', *, *, #475, .F. ) ;
#2098 = VERTEX_POINT ( 'NONE', #9771 ) ;
#2099 = ORIENTED_EDGE ( 'NONE', *, *, #12865, .T. ) ;
#2100 = EDGE_CURVE ( 'NONE', #3078, #10779, #19842, .T. ) ;
#2101 = CARTESIAN_POINT ( 'NONE',  ( 63.15554463217812042, 234.5677573683057062, -8.999999999999973355 ) ) ;
#2102 = CARTESIAN_POINT ( 'NONE',  ( 226.5610088730531686, 41.97375516554125596, -11.25902728360930638 ) ) ;
#2103 = CARTESIAN_POINT ( 'NONE',  ( 208.8107687779841228, 4.427644383670616079, -14.00000000000005507 ) ) ;
#2104 = EDGE_LOOP ( 'NONE', ( #1183, #10709, #4662, #6785 ) ) ;
#2105 = CARTESIAN_POINT ( 'NONE',  ( 48.16104799571871098, 210.5389873765740560, 45.89527237623691747 ) ) ;
#2106 = DIRECTION ( 'NONE',  ( 0.4953429730181650448, -0.8579591964396832138, -0.1361666490962400444 ) ) ;
#2107 = EDGE_LOOP ( 'NONE', ( #8715, #203, #20384 ) ) ;
#2108 = CARTESIAN_POINT ( 'NONE',  ( 64.01452848080103308, 153.0799536996103996, 56.00000000000000711 ) ) ;
#2109 = AXIS2_PLACEMENT_3D ( 'NONE', #7229, #13712, #20164 ) ;
#2110 = EDGE_CURVE ( 'NONE', #2016, #10851, #18262, .T. ) ;
#2111 = CONICAL_SURFACE ( 'NONE', #13969, 11.50000000000002309, 0.7853981633974477239 ) ;
#2112 = DIRECTION ( 'NONE',  ( -0.8645602258681719388, -0.4991540791356394169, -0.05814482891046558050 ) ) ;
#2113 = CARTESIAN_POINT ( 'NONE',  ( -27.31833330065622434, 51.55613243686521940, -5.649883545827639075 ) ) ;
#2114 = CARTESIAN_POINT ( 'NONE',  ( 206.2878473285719281, 10.21703256791452041, -1.872710068124176841 ) ) ;
#2115 = DIRECTION ( 'NONE',  ( -0.5000000000000054401, 0.8660254037844354880, -0.000000000000000000 ) ) ;
#2116 = DIRECTION ( 'NONE',  ( 0.5000000000000054401, -0.8660254037844354880, 0.000000000000000000 ) ) ;
#2118 = ORIENTED_EDGE ( 'NONE', *, *, #20369, .T. ) ;
#2117 = ORIENTED_EDGE ( 'NONE', *, *, #6280, .T. ) ;
#2119 = ORIENTED_EDGE ( 'NONE', *, *, #10172, .T. ) ;
#2120 = CARTESIAN_POINT ( 'NONE',  ( 60.24514846279297586, 84.21671670512185415, -17.09502645871620885 ) ) ;
#2121 = EDGE_CURVE ( 'NONE', #18641, #13417, #8613, .T. ) ;
#2122 = EDGE_LOOP ( 'NONE', ( #5272, #18553 ) ) ;
#2123 = EDGE_CURVE ( 'NONE', #7107, #10758, #6797, .T. ) ;
#2124 = ORIENTED_EDGE ( 'NONE', *, *, #17591, .F. ) ;
#2125 = CARTESIAN_POINT ( 'NONE',  ( 218.6326489791658503, 10.87112965241456841, -18.25196083293883120 ) ) ;
#2126 = AXIS2_PLACEMENT_3D ( 'NONE', #5501, #18134, #3606 ) ;
#2127 = VECTOR ( 'NONE', #20616, 1000.000000000000114 ) ;
#2128 = ORIENTED_EDGE ( 'NONE', *, *, #4038, .F. ) ;
#2129 = LINE ( 'NONE', #14865, #7674 ) ;
#2130 = CARTESIAN_POINT ( 'NONE',  ( 74.99529059433412215, 194.0607158131436165, 11.00000000000001066 ) ) ;
#2131 = EDGE_CURVE ( 'NONE', #4355, #3665, #15432, .T. ) ;
#2132 = VERTEX_POINT ( 'NONE', #11909 ) ;
#2133 = LINE ( 'NONE', #2022, #12853 ) ;
#2134 = DIRECTION ( 'NONE',  ( 0.000000000000000000, 0.000000000000000000, -1.000000000000000000 ) ) ;
#2135 = DIRECTION ( 'NONE',  ( 1.000000000000000000, 0.000000000000000000, 0.000000000000000000 ) ) ;
#2136 = CARTESIAN_POINT ( 'NONE',  ( 230.0028948683516603, 36.33870282379082539, -12.85003623376113069 ) ) ;
#2137 = CARTESIAN_POINT ( 'NONE',  ( 195.6285356662269237, 4.239886014466930142, -11.24974199967268618 ) ) ;
#2138 = VECTOR ( 'NONE', #10774, 1000.000000000000227 ) ;
#2139 = EDGE_CURVE ( 'NONE', #9246, #14150, #11695, .T. ) ;
#2140 = DIRECTION ( 'NONE',  ( -1.000000000000000000, -0.000000000000000000, -0.000000000000000000 ) ) ;
#2141 = CARTESIAN_POINT ( 'NONE',  ( 32.39721438298033007, 261.8427481158985302, -22.00000000000000355 ) ) ;
#2142 = DIRECTION ( 'NONE',  ( 0.5000000000000047740, -0.8660254037844359321, 0.000000000000000000 ) ) ;
#2143 = VERTEX_POINT ( 'NONE', #16569 ) ;
#2144 = CARTESIAN_POINT ( 'NONE',  ( 82.25469362684589214, 61.96434487962967808, 0.1446237860341569037 ) ) ;
#2145 = EDGE_CURVE ( 'NONE', #4987, #1053, #18374, .T. ) ;
#2146 = CARTESIAN_POINT ( 'NONE',  ( -14.77002974211693953, 71.43993639942684126, -4.849479976237960344 ) ) ;
#2147 = CARTESIAN_POINT ( 'NONE',  ( 78.60734359744111543, 53.30791790663061391, -6.696939495182443025 ) ) ;
#2149 = ORIENTED_EDGE ( 'NONE', *, *, #10776, .T. ) ;
#2148 = EDGE_LOOP ( 'NONE', ( #6519, #11364, #16039, #18985 ) ) ;
#2150 = EDGE_CURVE ( 'NONE', #5345, #470, #4301, .T. ) ;
#2151 = EDGE_LOOP ( 'NONE', ( #15487, #12873, #8459, #9810, #18958 ) ) ;
#2152 = CARTESIAN_POINT ( 'NONE',  ( 226.0260823154428067, 42.24727832654306070, -16.48323849494058635 ) ) ;
#2153 = EDGE_CURVE ( 'NONE', #3073, #7189, #13609, .T. ) ;
#2154 = EDGE_LOOP ( 'NONE', ( #10992, #18674, #1110, #16450 ) ) ;
#2155 = CARTESIAN_POINT ( 'NONE',  ( 77.73754876681609005, 55.65438722760616486, -3.442927121160782367 ) ) ;
#2156 = CARTESIAN_POINT ( 'NONE',  ( 10.00000000000000178, 0.000000000000000000, 0.000000000000000000 ) ) ;
#2157 = CARTESIAN_POINT ( 'NONE',  ( 211.5875185857062206, 6.803621723274593691, -25.94618751764496878 ) ) ;
#2158 = CARTESIAN_POINT ( 'NONE',  ( 218.4113082942438666, 37.92942609890246786, -15.81459191843834944 ) ) ;
#2159 = ORIENTED_EDGE ( 'NONE', *, *, #2669, .F. ) ;
#2160 = CARTESIAN_POINT ( 'NONE',  ( 219.2049426021622764, 11.20154352970703471, -12.53629070788368338 ) ) ;
#2161 = EDGE_CURVE ( 'NONE', #16889, #14507, #3838, .T. ) ;
#2162 = CARTESIAN_POINT ( 'NONE',  ( 202.1791022559531541, 13.45620526910691694, -14.00000000000008527 ) ) ;
#2163 = CARTESIAN_POINT ( 'NONE',  ( -31.82323003959540486, 64.25000000000000000, 2.481238266578627449 ) ) ;
#2164 = ORIENTED_EDGE ( 'NONE', *, *, #20773, .F. ) ;
#2165 = CIRCLE ( 'NONE', #5181, 8.000000000000058620 ) ;
#2166 = CIRCLE ( 'NONE', #13339, 3.902363844300875240 ) ;
#2167 = FILL_AREA_STYLE ('',( #13094 ) ) ;
#2168 = LINE ( 'NONE', #8619, #17284 ) ;
#2169 = DIRECTION ( 'NONE',  ( -0.5000000000000047740, 0.8660254037844358210, 0.000000000000000000 ) ) ;
#2170 = CARTESIAN_POINT ( 'NONE',  ( -1.416671275182913803, 79.14063577707194952, -7.486051927416997209 ) ) ;
#2171 = EDGE_CURVE ( 'NONE', #3291, #4535, #15006, .T. ) ;
#2173 = ORIENTED_EDGE ( 'NONE', *, *, #8855, .T. ) ;
#2172 = ORIENTED_EDGE ( 'NONE', *, *, #17565, .F. ) ;
#2174 = VERTEX_POINT ( 'NONE', #20064 ) ;
#2175 = DIRECTION ( 'NONE',  ( 0.000000000000000000, 0.000000000000000000, 1.000000000000000000 ) ) ;
#2176 = DIRECTION ( 'NONE',  ( -1.000000000000000000, -0.000000000000000000, -0.000000000000000000 ) ) ;
#2177 = CARTESIAN_POINT ( 'NONE',  ( 208.4761278624580711, 5.007259451653140125, -14.00000000000005507 ) ) ;
#2178 = EDGE_CURVE ( 'NONE', #19313, #10237, #16954, .T. ) ;
#2179 = DIRECTION ( 'NONE',  ( 0.5000000000000007772, -0.8660254037844381525, 0.000000000000000000 ) ) ;
#2180 = CARTESIAN_POINT ( 'NONE',  ( -26.51357854883240250, 5.755818230185494322, 6.781050089207113274 ) ) ;
#2181 = AXIS2_PLACEMENT_3D ( 'NONE', #850, #7300, #2761 ) ;
#2182 = CARTESIAN_POINT ( 'NONE',  ( 195.6699422177752581, 3.732742836357164862, -18.25196083293855054 ) ) ;
#2183 = ORIENTED_EDGE ( 'NONE', *, *, #17676, .T. ) ;
#2184 = CARTESIAN_POINT ( 'NONE',  ( 81.90911831446538827, 56.94440004289425872, -23.68671869826702547 ) ) ;
#2185 = CARTESIAN_POINT ( 'NONE',  ( -14.45130347081977895, 45.60283267264664175, -12.40976118032397579 ) ) ;
#2186 = ORIENTED_EDGE ( 'NONE', *, *, #16687, .T. ) ;
#2187 = LINE ( 'NONE', #20401, #9823 ) ;
#2188 = CARTESIAN_POINT ( 'NONE',  ( 1.337262051077171554, 52.04110715870329074, -4.937170952670085100 ) ) ;
#2189 = CARTESIAN_POINT ( 'NONE',  ( 0.7730453538337805908, 77.96698928858462807, -4.956659039178682669 ) ) ;
#2190 = DIRECTION ( 'NONE',  ( -0.8660254037844358210, -0.5000000000000049960, 0.000000000000000000 ) ) ;
#2191 = CARTESIAN_POINT ( 'NONE',  ( 217.5682316584538682, 37.87617127834120367, -14.91677899116112371 ) ) ;
#2192 = DIRECTION ( 'NONE',  ( -0.5000000000000051070, 0.8660254037844359321, -0.000000000000000000 ) ) ;
#2193 = VERTEX_POINT ( 'NONE', #7227 ) ;
#2194 = ORIENTED_EDGE ( 'NONE', *, *, #8580, .F. ) ;
#2195 = ORIENTED_EDGE ( 'NONE', *, *, #1632, .T. ) ;
#2196 = VECTOR ( 'NONE', #2051, 1000.000000000000114 ) ;
#2197 = DIRECTION ( 'NONE',  ( -0.4814586436739026754, 0.8339108325863923143, -0.2697967711570247729 ) ) ;
#2198 = PLANE ( 'NONE',  #15254 ) ;
#2199 = VERTEX_POINT ( 'NONE', #11799 ) ;
#2200 = VERTEX_POINT ( 'NONE', #5526 ) ;
#2201 = DIRECTION ( 'NONE',  ( -0.8660254037844361541, -0.5000000000000044409, 5.976026924694052093E-17 ) ) ;
#2202 = CARTESIAN_POINT ( 'NONE',  ( 30.10683012259193703, -10.00000000000000000, 0.000000000000000000 ) ) ;
#2203 = DIRECTION ( 'NONE',  ( 0.000000000000000000, 1.000000000000000000, 0.000000000000000000 ) ) ;
#2204 = ORIENTED_EDGE ( 'NONE', *, *, #3642, .F. ) ;
#2205 = CARTESIAN_POINT ( 'NONE',  ( 99.99529059433426426, 150.7594456239217777, 1.000000000000008438 ) ) ;
#2206 = CARTESIAN_POINT ( 'NONE',  ( -19.54313540116165271, 69.44160316133660160, -3.534893197518165664 ) ) ;
#2207 = ADVANCED_FACE ( 'NONE', ( #20160 ), #565, .F. ) ;
#2208 = DIRECTION ( 'NONE',  ( -0.5000000000000045519, 0.8660254037844360431, 0.000000000000000000 ) ) ;
#2209 = EDGE_CURVE ( 'NONE', #5382, #13116, #19946, .T. ) ;
#2210 = CONICAL_SURFACE ( 'NONE', #20476, 4.057500000000000107, 1.047197551196593857 ) ;
#2211 = LINE ( 'NONE', #16936, #10565 ) ;
#2212 = CARTESIAN_POINT ( 'NONE',  ( -26.24293131821966440, 50.67981595510417492, -7.209414086732143900 ) ) ;
#2213 = DIRECTION ( 'NONE',  ( 0.5000000000000054401, -0.8660254037844354880, 0.000000000000000000 ) ) ;
#2214 = ORIENTED_EDGE ( 'NONE', *, *, #8610, .T. ) ;
#2215 = CARTESIAN_POINT ( 'NONE',  ( 218.7490010597510945, 37.34452507169554991, -11.35524774226742650 ) ) ;
#2216 = CARTESIAN_POINT ( 'NONE',  ( 213.3559741392790556, 18.59882530632892994, -21.18305361806777398 ) ) ;
#2218 = ORIENTED_EDGE ( 'NONE', *, *, #19902, .F. ) ;
#2217 = ORIENTED_EDGE ( 'NONE', *, *, #7593, .T. ) ;
#2219 = CARTESIAN_POINT ( 'NONE',  ( 58.57279107162051446, 85.50235892223300027, -12.67366829707468057 ) ) ;
#2220 = ORIENTED_EDGE ( 'NONE', *, *, #16687, .F. ) ;
#2221 = VERTEX_POINT ( 'NONE', #16778 ) ;
#2222 = DIRECTION ( 'NONE',  ( -0.9987303135603804449, 0.000000000000000000, 0.05037619254751497799 ) ) ;
#2223 = CARTESIAN_POINT ( 'NONE',  ( 220.1325240088992814, 10.96426281393859981, -15.47241223420017775 ) ) ;
#2224 = EDGE_CURVE ( 'NONE', #13549, #1455, #17632, .T. ) ;
#2225 = AXIS2_PLACEMENT_3D ( 'NONE', #768, #10278, #10383 ) ;
#2226 = ORIENTED_EDGE ( 'NONE', *, *, #11032, .F. ) ;
#2227 = PLANE ( 'NONE',  #16840 ) ;
#2228 = ORIENTED_EDGE ( 'NONE', *, *, #7798, .T. ) ;
#2229 = CIRCLE ( 'NONE', #17467, 3.902363844300875240 ) ;
#2230 = CARTESIAN_POINT ( 'NONE',  ( 43.00000000000000000, 3.309499999999999886, 0.000000000000000000 ) ) ;
#2231 = ORIENTED_EDGE ( 'NONE', *, *, #8439, .T. ) ;
#2232 = CYLINDRICAL_SURFACE ( 'NONE', #13515, 13.50000000000000711 ) ;
#2233 = DIRECTION ( 'NONE',  ( -0.000000000000000000, 1.000000000000000000, -0.000000000000000000 ) ) ;
#2234 = EDGE_CURVE ( 'NONE', #5663, #14662, #1946, .T. ) ;
#2235 = ADVANCED_FACE ( 'NONE', ( #3526 ), #9968, .F. ) ;
#2236 = LINE ( 'NONE', #755, #6147 ) ;
#2237 = CARTESIAN_POINT ( 'NONE',  ( 214.9988779556950078, 8.000350883196837515, -23.57241037536588735 ) ) ;
#2238 = DIRECTION ( 'NONE',  ( -0.8426815769442687065, -0.4865224352899185645, -0.2306158707424266763 ) ) ;
#2239 = VERTEX_POINT ( 'NONE', #7427 ) ;
#2240 = CARTESIAN_POINT ( 'NONE',  ( -28.91711977134676204, 72.10661837392655116, 0.7232648427664161161 ) ) ;
#2241 = DIRECTION ( 'NONE',  ( 0.5000000000000054401, -0.8660254037844354880, 0.000000000000000000 ) ) ;
#2242 = CARTESIAN_POINT ( 'NONE',  ( 10.49211908931699178, -24.14213562373095456, 5.000000000000000000 ) ) ;
#2243 = AXIS2_PLACEMENT_3D ( 'NONE', #17924, #1807, #14758 ) ;
#2244 = VERTEX_POINT ( 'NONE', #9327 ) ;
#2245 = VECTOR ( 'NONE', #4734, 1000.000000000000000 ) ;
#2246 = CARTESIAN_POINT ( 'NONE',  ( 78.30707807390135144, 56.45514055384987984, -2.690560523447495633 ) ) ;
#2247 = VERTEX_POINT ( 'NONE', #2683 ) ;
#2248 = DIRECTION ( 'NONE',  ( -0.5000000000000051070, 0.8660254037844359321, -0.000000000000000000 ) ) ;
#2249 = CARTESIAN_POINT ( 'NONE',  ( 77.08812400714005264, 54.76052789366846696, -4.475059266215096088 ) ) ;
#2251 = ORIENTED_EDGE ( 'NONE', *, *, #1479, .T. ) ;
#2250 = VERTEX_POINT ( 'NONE', #7646 ) ;
#2252 = DIRECTION ( 'NONE',  ( -0.7738141867167189769, -0.3917653205579255671, -0.4977263686445478896 ) ) ;
#2253 = CARTESIAN_POINT ( 'NONE',  ( 4.000000000000000000, 0.000000000000000000, 0.000000000000000000 ) ) ;
#2254 = EDGE_LOOP ( 'NONE', ( #10674, #19755, #8751, #5116, #17485 ) ) ;
#2255 = DIRECTION ( 'NONE',  ( 0.5000000000000051070, -0.8660254037844359321, 0.000000000000000000 ) ) ;
#2256 = CARTESIAN_POINT ( 'NONE',  ( -18.07811133437977347, 79.99981534483862333, -12.41883285859719344 ) ) ;
#2257 = CARTESIAN_POINT ( 'NONE',  ( 198.4369456227295245, 5.507295677492109576, -5.040853264743329731 ) ) ;
#2258 = DIRECTION ( 'NONE',  ( -0.8660254037844363761, -0.5000000000000043299, 6.872020471724002955E-17 ) ) ;
#2259 = VERTEX_POINT ( 'NONE', #4046 ) ;
#2260 = EDGE_CURVE ( 'NONE', #15541, #9504, #13815, .T. ) ;
#2261 = EDGE_CURVE ( 'NONE', #20843, #16845, #18974, .T. ) ;
#2262 = CARTESIAN_POINT ( 'NONE',  ( 208.0931370707057226, 4.270918748101473206, -26.10149651730435494 ) ) ;
#2263 = CARTESIAN_POINT ( 'NONE',  ( 209.9432949659958183, 27.24318779734733553, -12.53629070788368338 ) ) ;
#2264 = CARTESIAN_POINT ( 'NONE',  ( -11.10102051443364779, 16.09941697557071905, 0.9999999999999997780 ) ) ;
#2265 = ORIENTED_EDGE ( 'NONE', *, *, #15773, .F. ) ;
#2266 = CARTESIAN_POINT ( 'NONE',  ( -7.400583024429460366, 65.00000000000000000, -12.50000000000000000 ) ) ;
#2267 = DIRECTION ( 'NONE',  ( -0.8660254037844354880, -0.5000000000000055511, 0.000000000000000000 ) ) ;
#2268 = EDGE_CURVE ( 'NONE', #13099, #5375, #13227, .T. ) ;
#2269 = DIRECTION ( 'NONE',  ( 0.8660254037844370423, 0.5000000000000026645, -0.000000000000000000 ) ) ;
#2270 = CARTESIAN_POINT ( 'NONE',  ( -14.95778962878673823, 79.99997668367075221, -12.46941917154138579 ) ) ;
#2271 = VERTEX_POINT ( 'NONE', #17200 ) ;
#2272 = EDGE_LOOP ( 'NONE', ( #3905, #20020, #978 ) ) ;
#2273 = DIRECTION ( 'NONE',  ( -0.5000000000000034417, 0.8660254037844364872, 0.000000000000000000 ) ) ;
#2274 = CARTESIAN_POINT ( 'NONE',  ( 192.3204675648519242, 17.06864365341445477, -14.00000000000005507 ) ) ;
#2275 = CARTESIAN_POINT ( 'NONE',  ( 227.7861124192640432, 39.52532352243469660, -17.80134517191574872 ) ) ;
#2276 = B_SPLINE_CURVE_WITH_KNOTS ( 'NONE', 3,
 ( #12401, #17476, #9289, #5802 ),
 .UNSPECIFIED., .F., .F.,
 ( 4, 4 ),
 ( 2.009138858749454001E-05, 0.0005860176108828354024 ),
 .UNSPECIFIED. ) ;
#2277 = ORIENTED_EDGE ( 'NONE', *, *, #1587, .T. ) ;
#2278 = EDGE_CURVE ( 'NONE', #1760, #20025, #15627, .T. ) ;
#2279 = DIRECTION ( 'NONE',  ( 0.000000000000000000, 0.000000000000000000, -1.000000000000000000 ) ) ;
#2280 = CARTESIAN_POINT ( 'NONE',  ( -27.39280497843907369, 9.626916829668232367, 5.187444349353440565 ) ) ;
#2281 = LINE ( 'NONE', #5329, #17435 ) ;
#2282 = ORIENTED_EDGE ( 'NONE', *, *, #12369, .F. ) ;
#2283 = EDGE_CURVE ( 'NONE', #6933, #19358, #1301, .T. ) ;
#2284 = AXIS2_PLACEMENT_3D ( 'NONE', #10586, #5492, #636 ) ;
#2285 = CARTESIAN_POINT ( 'NONE',  ( 82.33150071157334082, 63.03942819492690575, -25.35471444149103348 ) ) ;
#2286 = CARTESIAN_POINT ( 'NONE',  ( 210.5718816476998256, 5.444423373074280370, -2.341985411377013548 ) ) ;
#2287 = APPLICATION_CONTEXT ( 'automotive_design' ) ;
#2288 = ORIENTED_EDGE ( 'NONE', *, *, #5357, .F. ) ;
#2289 = CARTESIAN_POINT ( 'NONE',  ( 27.33329038210763784, 65.74999999999995737, -2.193932927905871022 ) ) ;
#2290 = DIRECTION ( 'NONE',  ( 0.3886714912512189701, 0.2243995901002275584, -0.8936326403234180482 ) ) ;
#2291 = DIRECTION ( 'NONE',  ( 0.5000000000000051070, -0.8660254037844359321, 0.000000000000000000 ) ) ;
#2292 = EDGE_CURVE ( 'NONE', #9960, #734, #10615, .T. ) ;
#2293 = FACE_OUTER_BOUND ( 'NONE', #20113, .T. ) ;
#2294 = DIRECTION ( 'NONE',  ( -0.5000000000000034417, 0.8660254037844364872, 0.000000000000000000 ) ) ;
#2295 = CARTESIAN_POINT ( 'NONE',  ( 206.4681030732283205, 9.967063913005945963, -26.45271578590685380 ) ) ;
#2296 = EDGE_CURVE ( 'NONE', #3214, #5044, #12539, .T. ) ;
#2298 = ORIENTED_EDGE ( 'NONE', *, *, #10250, .T. ) ;
#2297 = VERTEX_POINT ( 'NONE', #1092 ) ;
#2299 = EDGE_LOOP ( 'NONE', ( #5299, #19836, #10972, #16721 ) ) ;
#2300 = VERTEX_POINT ( 'NONE', #16990 ) ;
#2301 = FACE_OUTER_BOUND ( 'NONE', #14390, .T. ) ;
#2302 = DIRECTION ( 'NONE',  ( -0.8660254037844360431, -0.5000000000000045519, -0.000000000000000000 ) ) ;
#2303 = VERTEX_POINT ( 'NONE', #17099 ) ;
#2304 = TOROIDAL_SURFACE ( 'NONE', #5312, 2.961423854602172501, 1.000000000000000000 ) ;
#2305 = PLANE ( 'NONE',  #19993 ) ;
#2306 = DIRECTION ( 'NONE',  ( -0.5000000000000051070, 0.8660254037844359321, -0.000000000000000000 ) ) ;
#2307 = VERTEX_POINT ( 'NONE', #2583 ) ;
#2308 = ADVANCED_FACE ( 'NONE', ( #12113 ), #18657, .T. ) ;
#2309 = AXIS2_PLACEMENT_3D ( 'NONE', #5495, #8995, #15497 ) ;
#2310 = FACE_OUTER_BOUND ( 'NONE', #12343, .T. ) ;
#2311 = CARTESIAN_POINT ( 'NONE',  ( 203.0861028855985069, 1.895327080324426428, -3.188775577416750995 ) ) ;
#2312 = ORIENTED_EDGE ( 'NONE', *, *, #2928, .T. ) ;
#2313 = CARTESIAN_POINT ( 'NONE',  ( 229.4623969809411506, 36.29540673510603455, -14.55761806292095706 ) ) ;
#2314 = ADVANCED_FACE ( 'NONE', ( #20372 ), #982, .T. ) ;
#2315 = B_SPLINE_CURVE_WITH_KNOTS ( 'NONE', 3,
 ( #3925, #15506, #1073, #759 ),
 .UNSPECIFIED., .F., .F.,
 ( 4, 4 ),
 ( 4.203583920150003484E-07, 0.0008544060963757356712 ),
 .UNSPECIFIED. ) ;
#2316 = VECTOR ( 'NONE', #7607, 1000.000000000000227 ) ;
#2317 = DIRECTION ( 'NONE',  ( 0.8660254037844372643, 0.5000000000000027756, -0.000000000000000000 ) ) ;
#2318 = CARTESIAN_POINT ( 'NONE',  ( -28.41012295193859316, 51.34328577455362108, 1.513759717780124747 ) ) ;
#2319 = AXIS2_PLACEMENT_3D ( 'NONE', #1178, #9418, #4561 ) ;
#2320 = DIRECTION ( 'NONE',  ( -0.8528685319524387243, -0.4924038765061080070, 0.1736481776669413502 ) ) ;
#2321 =( GEOMETRIC_REPRESENTATION_CONTEXT ( 3 ) GLOBAL_UNCERTAINTY_ASSIGNED_CONTEXT ( ( #10843 ) ) GLOBAL_UNIT_ASSIGNED_CONTEXT ( ( #20398, #10971, #10854 ) ) REPRESENTATION_CONTEXT ( 'NONE', 'WORKASPACE' ) );
#2322 = FACE_OUTER_BOUND ( 'NONE', #2755, .T. ) ;
#2323 = DIRECTION ( 'NONE',  ( 0.8660254037844370423, 0.5000000000000026645, -0.000000000000000000 ) ) ;
#2325 = VERTEX_POINT ( 'NONE', #7748 ) ;
#2324 = EDGE_LOOP ( 'NONE', ( #15752, #3083, #16575, #7086 ) ) ;
#2326 = CARTESIAN_POINT ( 'NONE',  ( 59.78152309849413371, 84.57340574088013341, -16.44406699097515911 ) ) ;
#2327 = ORIENTED_EDGE ( 'NONE', *, *, #16127, .F. ) ;
#2328 = EDGE_LOOP ( 'NONE', ( #19910, #7756, #15014, #18546 ) ) ;
#2329 = ORIENTED_EDGE ( 'NONE', *, *, #20256, .T. ) ;
#2330 = VERTEX_POINT ( 'NONE', #10823 ) ;
#2331 = DIRECTION ( 'NONE',  ( -0.5570505456811891687, 0.8304785906670257845, 1.221880113418482660E-16 ) ) ;
#2332 = CARTESIAN_POINT ( 'NONE',  ( 54.01452848080093361, 170.4004617752990498, 4.000000000000000000 ) ) ;
#2333 = CONICAL_SURFACE ( 'NONE', #19915, 4.057500000000029416, 1.047197551196593857 ) ;
#2334 = ORIENTED_EDGE ( 'NONE', *, *, #10697, .F. ) ;
#2335 = ORIENTED_EDGE ( 'NONE', *, *, #4367, .F. ) ;
#2336 = CARTESIAN_POINT ( 'NONE',  ( 9.014528480800532151, 248.3427481158983596, -28.99999999999997513 ) ) ;
#2337 = ORIENTED_EDGE ( 'NONE', *, *, #4832, .F. ) ;
#2338 = ORIENTED_EDGE ( 'NONE', *, *, #6587, .T. ) ;
#2339 = CARTESIAN_POINT ( 'NONE',  ( 214.9458835816058979, 7.969754567050957306, -23.47937149798938350 ) ) ;
#2340 = LINE ( 'NONE', #9202, #6212 ) ;
#2341 = DIRECTION ( 'NONE',  ( 0.8660254037844375974, 0.5000000000000019984, 4.163336342344337520E-16 ) ) ;
#2342 = LINE ( 'NONE', #20452, #4135 ) ;
#2343 = CARTESIAN_POINT ( 'NONE',  ( 74.11964624731606932, 223.5773763115391262, -13.99999999999998757 ) ) ;
#2344 = DIRECTION ( 'NONE',  ( 0.5000000000000051070, -0.8660254037844355990, 0.000000000000000000 ) ) ;
#2345 = CARTESIAN_POINT ( 'NONE',  ( -33.44163564243958575, 75.56468634061936029, -1.801359935166299886 ) ) ;
#2346 = DIRECTION ( 'NONE',  ( -0.8660254037844355990, -0.5000000000000054401, 2.044166132021871316E-14 ) ) ;
#2347 = DIRECTION ( 'NONE',  ( 0.8660254037844360431, 0.5000000000000044409, -5.976026924694052093E-17 ) ) ;
#2348 = VECTOR ( 'NONE', #15597, 999.9999999999998863 ) ;
#2349 = VERTEX_POINT ( 'NONE', #2889 ) ;
#2350 = FACE_OUTER_BOUND ( 'NONE', #11102, .T. ) ;
#2351 = EDGE_LOOP ( 'NONE', ( #6381, #2897, #8936, #1401 ) ) ;
#2352 = DIRECTION ( 'NONE',  ( -0.5000000000000058842, 0.8660254037844351549, 0.000000000000000000 ) ) ;
#2353 = CARTESIAN_POINT ( 'NONE',  ( 80.96203380818354844, 54.00641746404563293, -3.266085604399942000 ) ) ;
#2354 = ADVANCED_FACE ( 'NONE', ( #13919 ), #9824, .T. ) ;
#2355 = DIRECTION ( 'NONE',  ( 0.000000000000000000, 0.000000000000000000, 1.000000000000000000 ) ) ;
#2356 = DIRECTION ( 'NONE',  ( -0.8000000000000001554, 0.000000000000000000, -0.5999999999999999778 ) ) ;
#2357 = VECTOR ( 'NONE', #15447, 1000.000000000000000 ) ;
#2358 = ORIENTED_EDGE ( 'NONE', *, *, #1732, .F. ) ;
#2359 = CARTESIAN_POINT ( 'NONE',  ( 80.58279200417960908, 59.94663314240338536, -24.49284399293752301 ) ) ;
#2360 = CARTESIAN_POINT ( 'NONE',  ( -18.07408198074340788, 79.99963191228553683, -12.37854261456184268 ) ) ;
#2361 = DIRECTION ( 'NONE',  ( 0.8660254037844355990, 0.5000000000000054401, 0.000000000000000000 ) ) ;
#2362 = CARTESIAN_POINT ( 'NONE',  ( 196.2195613929434899, 4.227088295528298900, -8.480087152951162111 ) ) ;
#2363 = ORIENTED_EDGE ( 'NONE', *, *, #7678, .T. ) ;
#2364 = CARTESIAN_POINT ( 'NONE',  ( 228.3459957934797728, 39.20853620448261978, -17.53429396590399492 ) ) ;
#2365 = ADVANCED_FACE ( 'NONE', ( #18899 ), #14950, .T. ) ;
#2366 = CARTESIAN_POINT ( 'NONE',  ( 217.5077365114557608, 9.448841045723993304, -22.49869731917979010 ) ) ;
#2367 = FACE_OUTER_BOUND ( 'NONE', #1220, .T. ) ;
#2368 = VERTEX_POINT ( 'NONE', #15734 ) ;
#2369 = CARTESIAN_POINT ( 'NONE',  ( 213.7874248973967610, 18.84792351767029572, -16.70797078425240656 ) ) ;
#2370 = DIRECTION ( 'NONE',  ( -0.8660254037844363761, -0.5000000000000043299, 6.872020471724002955E-17 ) ) ;
#2371 = DIRECTION ( 'NONE',  ( 0.5000000000000052180, -0.8660254037844355990, -0.000000000000000000 ) ) ;
#2372 = CARTESIAN_POINT ( 'NONE',  ( 226.3064090010233258, 42.74120415546374119, -16.68624095904336357 ) ) ;
#2373 = EDGE_CURVE ( 'NONE', #13537, #7703, #14250, .T. ) ;
#2375 = EDGE_LOOP ( 'NONE', ( #14028, #11153, #4846, #6412 ) ) ;
#2374 = ORIENTED_EDGE ( 'NONE', *, *, #11065, .T. ) ;
#2376 = VECTOR ( 'NONE', #276, 1000.000000000000000 ) ;
#2377 = ORIENTED_EDGE ( 'NONE', *, *, #10708, .F. ) ;
#2378 = EDGE_CURVE ( 'NONE', #20835, #4202, #7328, .T. ) ;
#2379 = CARTESIAN_POINT ( 'NONE',  ( 228.5767221322753073, 38.80890646304447955, -10.64970491435236077 ) ) ;
#2380 = DIRECTION ( 'NONE',  ( -0.8660254037844360431, -0.5000000000000044409, 5.976026924694052093E-17 ) ) ;
#2381 = CARTESIAN_POINT ( 'NONE',  ( 219.0841311483638947, 10.35897291369198747, -15.40190399002830723 ) ) ;
#2382 = CARTESIAN_POINT ( 'NONE',  ( 82.95222531821094947, 62.25068779409587449, -25.39145899207881030 ) ) ;
#2383 = CARTESIAN_POINT ( 'NONE',  ( -28.41032686606757096, 6.478790711288843873, 1.559431153037987849 ) ) ;
#2384 = LINE ( 'NONE', #15235, #4553 ) ;
#2385 = VERTEX_POINT ( 'NONE', #6048 ) ;
#2386 = ADVANCED_FACE ( 'NONE', ( #18579 ), #12960, .F. ) ;
#2387 = CARTESIAN_POINT ( 'NONE',  ( 81.35960895894935163, 61.54332286617361802, -25.03457989382592430 ) ) ;
#2388 = AXIS2_PLACEMENT_3D ( 'NONE', #16265, #153, #8293 ) ;
#2389 = CARTESIAN_POINT ( 'NONE',  ( 64.18815039242018372, 81.17459403355988456, -20.61608748715355333 ) ) ;
#2390 = CIRCLE ( 'NONE', #1034, 5.000000000000000888 ) ;
#2391 = ORIENTED_EDGE ( 'NONE', *, *, #14474, .F. ) ;
#2392 = DIRECTION ( 'NONE',  ( 0.8660254037844355990, 0.5000000000000054401, 0.000000000000000000 ) ) ;
#2393 = DIRECTION ( 'NONE',  ( 0.8660254037844374864, 0.5000000000000018874, 8.326672684688672821E-17 ) ) ;
#2394 = EDGE_CURVE ( 'NONE', #4803, #4463, #14455, .T. ) ;
#2395 = LINE ( 'NONE', #5765, #14247 ) ;
#2396 = DIRECTION ( 'NONE',  ( -0.8660254037844360431, -0.5000000000000045519, -4.336808689942049784E-16 ) ) ;
#2397 = CARTESIAN_POINT ( 'NONE',  ( 227.5312376355471145, 39.64027283883993391, -14.00000000000005507 ) ) ;
#2399 = ORIENTED_EDGE ( 'NONE', *, *, #5489, .T. ) ;
#2398 = VERTEX_POINT ( 'NONE', #14355 ) ;
#2400 = ORIENTED_EDGE ( 'NONE', *, *, #10149, .T. ) ;
#2401 = CARTESIAN_POINT ( 'NONE',  ( 209.4254563108873413, 4.782534396259798370, -2.075899210536075401 ) ) ;
#2402 = CARTESIAN_POINT ( 'NONE',  ( 203.0627220339503936, 1.881828139331499727, -24.79563718815128226 ) ) ;
#2403 = EDGE_CURVE ( 'NONE', #18303, #10779, #16141, .T. ) ;
#2404 = VECTOR ( 'NONE', #96, 1000.000000000000227 ) ;
#2405 = EDGE_LOOP ( 'NONE', ( #13727, #14907, #5786, #20302, #5911 ) ) ;
#2406 = LINE ( 'NONE', #15050, #8892 ) ;
#2407 = LINE ( 'NONE', #8658, #8146 ) ;
#2408 = AXIS2_PLACEMENT_3D ( 'NONE', #14730, #183, #14520 ) ;
#2409 = CARTESIAN_POINT ( 'NONE',  ( 173.9132435853527454, 54.87193107572242212, -14.00000000000002842 ) ) ;
#2410 = CIRCLE ( 'NONE', #14943, 4.999999999999978684 ) ;
#2411 = DIRECTION ( 'NONE',  ( -0.8601696498176563122, -0.4966191788709776733, -0.1160929141252233648 ) ) ;
#2412 = FACE_OUTER_BOUND ( 'NONE', #9581, .T. ) ;
#2413 = CIRCLE ( 'NONE', #11239, 3.902363844300875240 ) ;
#2414 = EDGE_CURVE ( 'NONE', #16240, #8157, #16622, .T. ) ;
#2415 = ORIENTED_EDGE ( 'NONE', *, *, #11750, .F. ) ;
#2416 = EDGE_CURVE ( 'NONE', #19916, #3954, #4771, .T. ) ;
#2417 = CARTESIAN_POINT ( 'NONE',  ( 229.7450441735844322, 36.78531332789425079, -14.53826389233656968 ) ) ;
#2418 = CIRCLE ( 'NONE', #1078, 3.902363844300875240 ) ;
#2419 = DIRECTION ( 'NONE',  ( -1.000000000000000000, -0.000000000000000000, -0.000000000000000000 ) ) ;
#2420 = CARTESIAN_POINT ( 'NONE',  ( -25.43178678872172682, 45.02209116438434933, -8.210452674424425723 ) ) ;
#2421 = DIRECTION ( 'NONE',  ( 1.000000000000000000, 0.000000000000000000, 0.000000000000000000 ) ) ;
#2422 = CIRCLE ( 'NONE', #20695, 3.619616396367202782 ) ;
#2423 = ADVANCED_FACE ( 'NONE', ( #9545 ), #20784, .T. ) ;
#2424 = ORIENTED_EDGE ( 'NONE', *, *, #16699, .T. ) ;
#2425 = CARTESIAN_POINT ( 'NONE',  ( 9.999999999999998224, 0.000000000000000000, 0.000000000000000000 ) ) ;
#2426 = CIRCLE ( 'NONE', #14296, 12.47473710546057823 ) ;
#2427 = CARTESIAN_POINT ( 'NONE',  ( -28.37382670920847971, 51.80430336678647762, 1.824942738421546862 ) ) ;
#2429 = EDGE_LOOP ( 'NONE', ( #1493, #12041, #20542, #18730, #10468, #7009 ) ) ;
#2428 = ORIENTED_EDGE ( 'NONE', *, *, #17412, .F. ) ;
#2430 = CARTESIAN_POINT ( 'NONE',  ( 172.3972143829816162, 19.35563505625646030, -19.00000000000000355 ) ) ;
#2431 = CARTESIAN_POINT ( 'NONE',  ( 58.88264075909191320, 85.26433268085669681, -14.50872457446225461 ) ) ;
#2432 = ORIENTED_EDGE ( 'NONE', *, *, #4613, .T. ) ;
#2433 = ORIENTED_EDGE ( 'NONE', *, *, #20050, .T. ) ;
#2434 = DIRECTION ( 'NONE',  ( 0.000000000000000000, -1.000000000000000000, 0.000000000000000000 ) ) ;
#2435 = DIRECTION ( 'NONE',  ( 0.5000000000000054401, -0.8660254037844354880, 0.000000000000000000 ) ) ;
#2436 = ADVANCED_FACE ( 'NONE', ( #1608 ), #9435, .T. ) ;
#2437 = ORIENTED_EDGE ( 'NONE', *, *, #17027, .T. ) ;
#2438 = ORIENTED_EDGE ( 'NONE', *, *, #10250, .F. ) ;
#2439 = CARTESIAN_POINT ( 'NONE',  ( 207.6891655446386551, 10.67204465957205350, -26.28791492288521781 ) ) ;
#2440 = ORIENTED_EDGE ( 'NONE', *, *, #20218, .F. ) ;
#2441 = AXIS2_PLACEMENT_3D ( 'NONE', #6995, #10484, #12205 ) ;
#2442 = VECTOR ( 'NONE', #7671, 1000.000000000000227 ) ;
#2443 = EDGE_CURVE ( 'NONE', #9834, #16454, #3098, .T. ) ;
#2444 = LINE ( 'NONE', #2758, #8385 ) ;
#2445 = VECTOR ( 'NONE', #15907, 1000.000000000000114 ) ;
#2446 = CARTESIAN_POINT ( 'NONE',  ( 30.10683012259193703, -10.00000000000000000, 0.000000000000000000 ) ) ;
#2447 = LINE ( 'NONE', #10914, #18245 ) ;
#2448 = AXIS2_PLACEMENT_3D ( 'NONE', #781, #7331, #15112 ) ;
#2449 = DIRECTION ( 'NONE',  ( 0.000000000000000000, 0.8660254037844381525, -0.5000000000000009992 ) ) ;
#2450 = CARTESIAN_POINT ( 'NONE',  ( 5.000000000000004441, -2.342598717236899830, 4.057500000000059615 ) ) ;
#2451 = LINE ( 'NONE', #10695, #4148 ) ;
#2452 = VERTEX_POINT ( 'NONE', #16044 ) ;
#2453 = CARTESIAN_POINT ( 'NONE',  ( -32.63107789565361117, 71.62317011047271365, 0.9609777548053090035 ) ) ;
#2454 = LINE ( 'NONE', #14230, #14712 ) ;
#2455 = CARTESIAN_POINT ( 'NONE',  ( 42.30949999999999989, 4.898587196589411843E-16, -3.999999999999999112 ) ) ;
#2456 = ORIENTED_EDGE ( 'NONE', *, *, #16016, .T. ) ;
#2457 = AXIS2_PLACEMENT_3D ( 'NONE', #2977, #15913, #10923 ) ;
#2458 = VECTOR ( 'NONE', #8371, 1000.000000000000114 ) ;
#2459 = CARTESIAN_POINT ( 'NONE',  ( -4.234137110339535326, 65.75000000000001421, 4.519411796990935315 ) ) ;
#2460 = AXIS2_PLACEMENT_3D ( 'NONE', #6433, #16521, #11434 ) ;
#2461 = B_SPLINE_CURVE_WITH_KNOTS ( 'NONE', 3,
 ( #7488, #12387, #4000, #16933 ),
 .UNSPECIFIED., .F., .F.,
 ( 4, 4 ),
 ( 2.042725466720964897E-07, 0.0005856926282862834213 ),
 .UNSPECIFIED. ) ;
#2462 = ORIENTED_EDGE ( 'NONE', *, *, #1234, .F. ) ;
#2463 = LINE ( 'NONE', #5512, #9142 ) ;
#2464 = CARTESIAN_POINT ( 'NONE',  ( 79.78989234911249184, 55.62452637193754867, -3.470983589548607640 ) ) ;
#2465 = DIRECTION ( 'NONE',  ( 0.8660254037844361541, 0.5000000000000045519, -5.976026924694053325E-17 ) ) ;
#2466 = CARTESIAN_POINT ( 'NONE',  ( 0.000000000000000000, 4.510281037539699062E-17, 6.500000000000047962 ) ) ;
#2467 = ORIENTED_EDGE ( 'NONE', *, *, #3686, .F. ) ;
#2468 = CARTESIAN_POINT ( 'NONE',  ( 211.7141293194486025, 6.361499597646727011, -2.388950188371981032 ) ) ;
#2469 = CARTESIAN_POINT ( 'NONE',  ( 5.000000000000000000, -4.685197434473809430, 6.071532165918824830E-15 ) ) ;
#2470 = AXIS2_PLACEMENT_3D ( 'NONE', #14671, #128, #16344 ) ;
#2471 = CARTESIAN_POINT ( 'NONE',  ( 218.9076280839623223, 35.55626861788439896, -17.48830818005195908 ) ) ;
#2472 = DIRECTION ( 'NONE',  ( -0.5000000000000054401, 0.8660254037844354880, -0.000000000000000000 ) ) ;
#2473 = ORIENTED_EDGE ( 'NONE', *, *, #20493, .F. ) ;
#2474 = VECTOR ( 'NONE', #19048, 1000.000000000000114 ) ;
#2475 = DIRECTION ( 'NONE',  ( -0.4272097022732466165, 0.7399489098236303741, -0.5195839500354345608 ) ) ;
#2476 =( BOUNDED_CURVE ( )  B_SPLINE_CURVE ( 3, ( #8745, #4299, #15659, #5761 ),
 .UNSPECIFIED., .F., .F. ) 
 B_SPLINE_CURVE_WITH_KNOTS ( ( 4, 4 ),
 ( 1.383924152946250041, 1.570796326794896558 ),
 .UNSPECIFIED. ) 
 CURVE ( )  GEOMETRIC_REPRESENTATION_ITEM ( )  RATIONAL_B_SPLINE_CURVE ( ( 1.000000000000000000, 0.9970920157757051649, 0.9970920157757051649, 1.000000000000000000 ) ) 
 REPRESENTATION_ITEM ( '' )  );
#2477 = DIRECTION ( 'NONE',  ( 0.1005394128318209540, 0.05804645706261960664, 0.9932383577419421350 ) ) ;
#2478 = ADVANCED_FACE ( 'NONE', ( #8049 ), #6456, .T. ) ;
#2479 = DIRECTION ( 'NONE',  ( 0.000000000000000000, 6.938893903907178303E-18, 1.000000000000000000 ) ) ;
#2481 = B_SPLINE_CURVE_WITH_KNOTS ( 'NONE', 3,
 ( #16304, #11214, #9605, #1880 ),
 .UNSPECIFIED., .F., .F.,
 ( 4, 4 ),
 ( 2.845336965508513413E-07, 0.0004523377754763962351 ),
 .UNSPECIFIED. ) ;
#2480 = PRODUCT_DEFINITION_SHAPE ( 'NONE', 'NONE',  #11897 ) ;
#2482 = ORIENTED_EDGE ( 'NONE', *, *, #20787, .T. ) ;
#2483 = CARTESIAN_POINT ( 'NONE',  ( 0.3999999999999975797, 0.000000000000000000, 0.000000000000000000 ) ) ;
#2484 = CARTESIAN_POINT ( 'NONE',  ( -4.701390418375630986, 65.75000000000000000, 5.347094680480811490 ) ) ;
#2485 = LINE ( 'NONE', #7338, #20363 ) ;
#2486 = CARTESIAN_POINT ( 'NONE',  ( 212.6158184066919716, 14.04749827747483693, -22.62267072728679906 ) ) ;
#2487 = AXIS2_PLACEMENT_3D ( 'NONE', #18427, #15476, #12068 ) ;
#2489 = ORIENTED_EDGE ( 'NONE', *, *, #3198, .T. ) ;
#2488 = ORIENTED_EDGE ( 'NONE', *, *, #3032, .F. ) ;
#2490 = CARTESIAN_POINT ( 'NONE',  ( 205.6550139379351663, 24.76734759143572262, -24.01557619556987788 ) ) ;
#2491 = CARTESIAN_POINT ( 'NONE',  ( 211.7681187495013830, 6.135071185814040540, -2.669358488461178069 ) ) ;
#2492 = ORIENTED_EDGE ( 'NONE', *, *, #15628, .T. ) ;
#2493 = EDGE_CURVE ( 'NONE', #6314, #20898, #21, .T. ) ;
#2494 = FACE_OUTER_BOUND ( 'NONE', #20816, .T. ) ;
#2495 = ORIENTED_EDGE ( 'NONE', *, *, #16978, .F. ) ;
#2496 = CARTESIAN_POINT ( 'NONE',  ( -28.48629072751340630, 8.589818999910622921, -0.6763375131893898384 ) ) ;
#2497 = CYLINDRICAL_SURFACE ( 'NONE', #8268, 4.999999999999975131 ) ;
#2498 = ORIENTED_EDGE ( 'NONE', *, *, #18453, .F. ) ;
#2499 = ADVANCED_BREP_SHAPE_REPRESENTATION ( '', ( #17599, #18233 ), #10424 ) ;
#2500 = CARTESIAN_POINT ( 'NONE',  ( 219.0136128684463870, 10.31825916579886382, -8.145074743996644884 ) ) ;
#2501 = AXIS2_PLACEMENT_3D ( 'NONE', #2446, #4136, #16855 ) ;
#2502 = CARTESIAN_POINT ( 'NONE',  ( 205.6089461623839441, 14.12607661844890039, -25.65046807331635748 ) ) ;
#2503 = AXIS2_PLACEMENT_3D ( 'NONE', #12544, #7650, #2794 ) ;
#2504 = EDGE_CURVE ( 'NONE', #10290, #206, #8156, .T. ) ;
#2505 = VERTEX_POINT ( 'NONE', #11260 ) ;
#2506 = EDGE_CURVE ( 'NONE', #17966, #10243, #16278, .T. ) ;
#2507 = FACE_OUTER_BOUND ( 'NONE', #16197, .T. ) ;
#2508 = DIRECTION ( 'NONE',  ( -0.000000000000000000, -1.000000000000000000, 0.000000000000000000 ) ) ;
#2509 = CARTESIAN_POINT ( 'NONE',  ( 217.9776690748798558, 9.720156737717866591, -19.29168348739315775 ) ) ;
#2510 = CARTESIAN_POINT ( 'NONE',  ( 199.4574108924007305, -0.1996992187545574282, -7.132002368301175288 ) ) ;
#2511 = FACE_OUTER_BOUND ( 'NONE', #7028, .T. ) ;
#2512 = EDGE_LOOP ( 'NONE', ( #9063, #19931, #4977, #17510, #11735 ) ) ;
#2513 = ORIENTED_EDGE ( 'NONE', *, *, #4834, .T. ) ;
#2514 = CARTESIAN_POINT ( 'NONE',  ( 177.1791022559528983, 56.75747545832873442, -29.00000000000007105 ) ) ;
#2515 = DIRECTION ( 'NONE',  ( 0.1997192025788092351, 0.1153079353712145594, -0.9730448705798270259 ) ) ;
#2516 = ORIENTED_EDGE ( 'NONE', *, *, #2504, .T. ) ;
#2517 = EDGE_LOOP ( 'NONE', ( #13399, #4945, #9576, #14159 ) ) ;
#2518 = CARTESIAN_POINT ( 'NONE',  ( 81.39009893423684616, 61.60396693986834293, 0.05555408759164950916 ) ) ;
#2519 = DIRECTION ( 'NONE',  ( -1.000000000000000000, -0.000000000000000000, -0.000000000000000000 ) ) ;
#2520 = DIRECTION ( 'NONE',  ( -1.000000000000000000, 0.000000000000000000, 0.000000000000000000 ) ) ;
#2521 = CARTESIAN_POINT ( 'NONE',  ( 205.8264633344831225, 9.596613037118636669, -14.00000000000005507 ) ) ;
#2522 = PRODUCT_RELATED_PRODUCT_CATEGORY ( 'part', '', ( #12121 ) ) ;
#2523 = CARTESIAN_POINT ( 'NONE',  ( 199.3931344365919927, 6.236368223744671369, -4.253719131806056986 ) ) ;
#2524 = EDGE_CURVE ( 'NONE', #9666, #18381, #19939, .T. ) ;
#2525 = CARTESIAN_POINT ( 'NONE',  ( 205.2117758015800462, 9.241723024529527208, -1.545471579934808215 ) ) ;
#2526 = EDGE_CURVE ( 'NONE', #772, #9185, #16908, .T. ) ;
#2527 = PLANE ( 'NONE',  #84 ) ;
#2528 = CARTESIAN_POINT ( 'NONE',  ( -21.63303579789734243, 49.55866895486145296, -11.18335248048085084 ) ) ;
#2529 = DIRECTION ( 'NONE',  ( 0.8660254037844360431, 0.5000000000000044409, -5.976026924694053325E-17 ) ) ;
#2530 = AXIS2_PLACEMENT_3D ( 'NONE', #10099, #10210, #3755 ) ;
#2531 = ADVANCED_FACE ( 'NONE', ( #3362 ), #12924, .T. ) ;
#2532 = DIRECTION ( 'NONE',  ( 0.5000000000000049960, -0.8660254037844358210, 0.000000000000000000 ) ) ;
#2533 = CARTESIAN_POINT ( 'NONE',  ( 218.3155656336024038, 36.58175086316158087, -17.77545290933957745 ) ) ;
#2535 = ORIENTED_EDGE ( 'NONE', *, *, #19238, .F. ) ;
#2534 = EDGE_LOOP ( 'NONE', ( #431, #7158, #8019, #1564 ) ) ;
#2536 = CARTESIAN_POINT ( 'NONE',  ( 201.8258408404966531, 26.51993709131365762, -13.80232238285611857 ) ) ;
#2537 = EDGE_CURVE ( 'NONE', #20176, #19523, #12107, .T. ) ;
#2538 = CARTESIAN_POINT ( 'NONE',  ( 63.99383217623863374, 81.32526156698924069, -20.50245894047660755 ) ) ;
#2539 = VERTEX_POINT ( 'NONE', #11222 ) ;
#2540 = EDGE_CURVE ( 'NONE', #456, #10779, #9612, .T. ) ;
#2541 = ORIENTED_EDGE ( 'NONE', *, *, #10632, .T. ) ;
#2542 = FACE_OUTER_BOUND ( 'NONE', #12900, .T. ) ;
#2543 = CARTESIAN_POINT ( 'NONE',  ( 1.111705572786244156, 51.52592968046116084, -5.897422193562015913 ) ) ;
#2544 = DIRECTION ( 'NONE',  ( -0.8660254037844355990, -0.5000000000000054401, -3.615531934188343626E-15 ) ) ;
#2545 = B_SPLINE_CURVE_WITH_KNOTS ( 'NONE', 3,
 ( #17127, #2616, #9057, #1018 ),
 .UNSPECIFIED., .F., .F.,
 ( 4, 4 ),
 ( 4.029077176330947946E-07, 0.0005663291300154840203 ),
 .UNSPECIFIED. ) ;
#2546 = VERTEX_POINT ( 'NONE', #16109 ) ;
#2547 = ORIENTED_EDGE ( 'NONE', *, *, #20248, .F. ) ;
#2548 = CARTESIAN_POINT ( 'NONE',  ( 212.7272071507568967, 14.11180859884542649, -5.291540431471497996 ) ) ;
#2549 = ADVANCED_FACE ( 'NONE', ( #8121 ), #20341, .F. ) ;
#2550 = CARTESIAN_POINT ( 'NONE',  ( 211.6495311407713018, 17.61360998178372483, -6.376588578941996488 ) ) ;
#2551 = CARTESIAN_POINT ( 'NONE',  ( 77.62926519054968821, 189.4985379866525648, 11.00000000000001066 ) ) ;
#2552 = AXIS2_PLACEMENT_3D ( 'NONE', #15146, #2192, #11834 ) ;
#2553 = LINE ( 'NONE', #7400, #4712 ) ;
#2554 = EDGE_CURVE ( 'NONE', #19224, #15951, #3261, .T. ) ;
#2555 = CARTESIAN_POINT ( 'NONE',  ( 80.00000000000000000, 2.894906536710095477E-17, 4.172000000000029907 ) ) ;
#2556 = DIRECTION ( 'NONE',  ( -0.8660254037844370423, -0.5000000000000026645, 0.000000000000000000 ) ) ;
#2557 = DIRECTION ( 'NONE',  ( 0.8660254037844370423, 0.5000000000000026645, -0.000000000000000000 ) ) ;
#2558 = EDGE_CURVE ( 'NONE', #10285, #1208, #19571, .T. ) ;
#2559 = VERTEX_POINT ( 'NONE', #4949 ) ;
#2560 = CARTESIAN_POINT ( 'NONE',  ( -28.86756580280676587, 70.94952981831229977, 1.317303739530243378 ) ) ;
#2561 = CARTESIAN_POINT ( 'NONE',  ( 205.8264633344831225, 9.596613037118636669, -14.00000000000005507 ) ) ;
#2562 = CARTESIAN_POINT ( 'NONE',  ( 226.7299261015226648, 42.00765101952459446, -17.47639052459119924 ) ) ;
#2563 = ORIENTED_EDGE ( 'NONE', *, *, #2669, .T. ) ;
#2564 = CIRCLE ( 'NONE', #5238, 12.47473710546057823 ) ;
#2565 = CARTESIAN_POINT ( 'NONE',  ( -3.601011660222551036, 65.75000000000000000, 3.829121630900767848 ) ) ;
#2566 = EDGE_CURVE ( 'NONE', #19041, #1588, #11424, .T. ) ;
#2567 = ORIENTED_EDGE ( 'NONE', *, *, #8251, .F. ) ;
#2568 = CIRCLE ( 'NONE', #1875, 15.00000000000001954 ) ;
#2569 = VERTEX_POINT ( 'NONE', #16311 ) ;
#2570 = LINE ( 'NONE', #10382, #374 ) ;
#2571 = AXIS2_PLACEMENT_3D ( 'NONE', #13843, #5653, #14253 ) ;
#2572 = DIRECTION ( 'NONE',  ( 0.000000000000000000, 0.000000000000000000, -1.000000000000000000 ) ) ;
#2573 = EDGE_CURVE ( 'NONE', #8298, #5808, #6631, .T. ) ;
#2574 = PRODUCT_CONTEXT ( 'NONE', #16373, 'mechanical' ) ;
#2575 = EDGE_CURVE ( 'NONE', #3665, #9396, #10168, .T. ) ;
#2576 = FACE_OUTER_BOUND ( 'NONE', #5270, .T. ) ;
#2577 = EDGE_LOOP ( 'NONE', ( #4212, #6761 ) ) ;
#2578 = CARTESIAN_POINT ( 'NONE',  ( 203.2433706042751282, 14.07066088650062241, -14.00000000000004974 ) ) ;
#2579 = ORIENTED_EDGE ( 'NONE', *, *, #4235, .F. ) ;
#2580 = CIRCLE ( 'NONE', #14438, 11.94520687646042667 ) ;
#2581 = CARTESIAN_POINT ( 'NONE',  ( 226.7180567368605182, 42.02820936217297998, -16.57782486433068669 ) ) ;
#2582 = CARTESIAN_POINT ( 'NONE',  ( 220.6367211117483009, 34.28081623197468986, -17.48404651990738046 ) ) ;
#2583 = CARTESIAN_POINT ( 'NONE',  ( 26.99999999999999645, 65.74999999999995737, -2.528164662410434804 ) ) ;
#2584 = AXIS2_PLACEMENT_3D ( 'NONE', #20465, #6345, #18889 ) ;
#2585 = DIRECTION ( 'NONE',  ( 0.000000000000000000, 0.000000000000000000, 1.000000000000000000 ) ) ;
#2586 = CIRCLE ( 'NONE', #20832, 3.902363844300875240 ) ;
#2587 = EDGE_CURVE ( 'NONE', #4599, #13568, #6268, .T. ) ;
#2588 = B_SPLINE_CURVE_WITH_KNOTS ( 'NONE', 3,
 ( #12668, #17749, #20803, #6273 ),
 .UNSPECIFIED., .F., .F.,
 ( 4, 4 ),
 ( 2.765582935491508733E-07, 0.0004523298000734451161 ),
 .UNSPECIFIED. ) ;
#2589 = DIRECTION ( 'NONE',  ( -0.5000000000000008882, 0.8660254037844381525, 0.000000000000000000 ) ) ;
#2590 = CARTESIAN_POINT ( 'NONE',  ( 205.8311783259423464, 2.707377034109388347, -2.561001429077326197 ) ) ;
#2591 = ORIENTED_EDGE ( 'NONE', *, *, #10824, .T. ) ;
#2592 = CARTESIAN_POINT ( 'NONE',  ( 226.5046556235327841, 42.39783093284840731, -10.88971489487116528 ) ) ;
#2593 = DIRECTION ( 'NONE',  ( 0.5000000000000027756, -0.8660254037844372643, 0.000000000000000000 ) ) ;
#2594 = CARTESIAN_POINT ( 'NONE',  ( 211.2164883113428857, 12.70854540844746872, -3.188775577416895324 ) ) ;
#2595 = DIRECTION ( 'NONE',  ( -0.8660254037844355990, -0.5000000000000054401, 2.044166132021871316E-14 ) ) ;
#2597 = ORIENTED_EDGE ( 'NONE', *, *, #12642, .F. ) ;
#2596 = VERTEX_POINT ( 'NONE', #16411 ) ;
#2598 = EDGE_LOOP ( 'NONE', ( #7297, #406, #4303, #13901, #13722 ) ) ;
#2599 = ORIENTED_EDGE ( 'NONE', *, *, #6392, .F. ) ;
#2600 = AXIS2_PLACEMENT_3D ( 'NONE', #15052, #7168, #18524 ) ;
#2601 = CARTESIAN_POINT ( 'NONE',  ( -12.02901256816104336, 12.04372001624153476, 11.85403899944298622 ) ) ;
#2602 = CARTESIAN_POINT ( 'NONE',  ( 10.49211908931699178, -10.00000000000000000, 5.000000000000000000 ) ) ;
#2603 = VECTOR ( 'NONE', #5241, 1000.000000000000000 ) ;
#2604 = EDGE_LOOP ( 'NONE', ( #4025, #9656 ) ) ;
#2605 = CARTESIAN_POINT ( 'NONE',  ( 221.6773453713352353, 32.27248394197634696, -14.91677899116122319 ) ) ;
#2606 = PRODUCT_DEFINITION_CONTEXT ( 'detailed design', #2972, 'design' ) ;
#2607 = CARTESIAN_POINT ( 'NONE',  ( 30.10683012259193703, 5.000000000000000000, 0.000000000000000000 ) ) ;
#2608 = CARTESIAN_POINT ( 'NONE',  ( -15.99999999999999289, 80.00000000000000000, 0.000000000000000000 ) ) ;
#2609 = FACE_OUTER_BOUND ( 'NONE', #13876, .T. ) ;
#2610 = CARTESIAN_POINT ( 'NONE',  ( 87.00490953756771262, 143.2594456239216925, 1.000000000000009326 ) ) ;
#2611 = ORIENTED_EDGE ( 'NONE', *, *, #17969, .F. ) ;
#2612 = AXIS2_PLACEMENT_3D ( 'NONE', #16479, #13312, #3747 ) ;
#2613 = LINE ( 'NONE', #7958, #17975 ) ;
#2614 = DIRECTION ( 'NONE',  ( 0.8660254037844360431, 0.5000000000000044409, -5.976026924694052093E-17 ) ) ;
#2615 = CARTESIAN_POINT ( 'NONE',  ( 208.0983737146324870, 5.661548828456886895, -14.00000000000005507 ) ) ;
#2616 = CARTESIAN_POINT ( 'NONE',  ( 228.0761299620636464, 39.02299840321953184, -17.72162118442982148 ) ) ;
#2617 = DIRECTION ( 'NONE',  ( 0.7951984747223628247, 0.4591080534401421609, 0.3960797660391544572 ) ) ;
#2618 = EDGE_CURVE ( 'NONE', #5028, #10237, #7474, .T. ) ;
#2619 = ORIENTED_EDGE ( 'NONE', *, *, #15165, .F. ) ;
#2620 = ORIENTED_EDGE ( 'NONE', *, *, #11484, .T. ) ;
#2621 = DIRECTION ( 'NONE',  ( -0.8660254037844357100, -0.5000000000000051070, 0.000000000000000000 ) ) ;
#2622 = ORIENTED_EDGE ( 'NONE', *, *, #11749, .T. ) ;
#2623 = EDGE_LOOP ( 'NONE', ( #220, #18273, #8127, #4405, #15092 ) ) ;
#2624 = CARTESIAN_POINT ( 'NONE',  ( -20.96748056867798837, 14.44039965061553410, 11.47079698816731685 ) ) ;
#2625 = CARTESIAN_POINT ( 'NONE',  ( 81.10655718899290889, 54.43739570252013493, -2.927339837283823520 ) ) ;
#2626 = CARTESIAN_POINT ( 'NONE',  ( 200.4142678326970213, 6.648903187691491468, -24.65893733905786078 ) ) ;
#2627 = FACE_OUTER_BOUND ( 'NONE', #9159, .T. ) ;
#2628 = VECTOR ( 'NONE', #3366, 1000.000000000000227 ) ;
#2629 = EDGE_CURVE ( 'NONE', #10364, #340, #12712, .T. ) ;
#2630 =( LENGTH_UNIT ( ) NAMED_UNIT ( * ) SI_UNIT ( .MILLI., .METRE. ) );
#2631 = ORIENTED_EDGE ( 'NONE', *, *, #15255, .T. ) ;
#2632 = CARTESIAN_POINT ( 'NONE',  ( 216.3683575532813848, 33.19538101841231992, -14.00000000000004441 ) ) ;
#2633 = LINE ( 'NONE', #10772, #19364 ) ;
#2634 = CARTESIAN_POINT ( 'NONE',  ( -15.66551832401957078, 45.63517971373708804, -12.50026680680302604 ) ) ;
#2635 = CARTESIAN_POINT ( 'NONE',  ( 207.5734976231972837, 16.57066088650062241, -14.00000000000004974 ) ) ;
#2636 = DIRECTION ( 'NONE',  ( -0.4330127018922106941, -0.2499999999999983347, 0.8660254037844433705 ) ) ;
#2637 = EDGE_CURVE ( 'NONE', #7254, #16403, #18320, .T. ) ;
#2638 = CARTESIAN_POINT ( 'NONE',  ( -28.28813791240392916, 47.26616069107360829, -2.314127915140642866 ) ) ;
#2640 = VERTEX_POINT ( 'NONE', #5354 ) ;
#2639 = ORIENTED_EDGE ( 'NONE', *, *, #12097, .T. ) ;
#2641 = DIRECTION ( 'NONE',  ( -0.5000000000000049960, 0.8660254037844357100, -0.000000000000000000 ) ) ;
#2642 = CARTESIAN_POINT ( 'NONE',  ( 221.0616351780288653, 31.82541889109742073, -14.53509620734056540 ) ) ;
#2643 = EDGE_LOOP ( 'NONE', ( #20461, #19681, #12372, #18310, #17007 ) ) ;
#2644 = VERTEX_POINT ( 'NONE', #8553 ) ;
#2645 = DIRECTION ( 'NONE',  ( 0.000000000000000000, 1.000000000000000000, 0.000000000000000000 ) ) ;
#2646 = CARTESIAN_POINT ( 'NONE',  ( 206.4249228987308413, 10.47318308942859133, -13.04168858804099784 ) ) ;
#2647 = CARTESIAN_POINT ( 'NONE',  ( -15.23524979826371073, 50.47648804990845406, -16.25068009060050400 ) ) ;
#2648 = CARTESIAN_POINT ( 'NONE',  ( -27.63586018514423515, 9.449117160379985947, -4.578843963689200436 ) ) ;
#2649 = ORIENTED_EDGE ( 'NONE', *, *, #11330, .F. ) ;
#2650 = EDGE_CURVE ( 'NONE', #7341, #1221, #7553, .T. ) ;
#2651 = VERTEX_POINT ( 'NONE', #13441 ) ;
#2652 = EDGE_CURVE ( 'NONE', #6933, #6371, #7285, .T. ) ;
#2653 = CARTESIAN_POINT ( 'NONE',  ( 219.6345796647896691, 34.29715154524891574, -10.49174204642378072 ) ) ;
#2654 = DIRECTION ( 'NONE',  ( -0.9659258262890694224, 0.2588190451025162431, 0.000000000000000000 ) ) ;
#2655 = CARTESIAN_POINT ( 'NONE',  ( 199.2231352798573027, 21.03391272677540513, -14.00000000000005507 ) ) ;
#2656 = CIRCLE ( 'NONE', #11787, 6.500000000000000000 ) ;
#2657 = PRODUCT_DEFINITION_SHAPE ( 'NONE', 'NONE',  #13142 ) ;
#2658 = DIRECTION ( 'NONE',  ( -0.8660254037844357100, -0.5000000000000049960, 0.000000000000000000 ) ) ;
#2659 = CONICAL_SURFACE ( 'NONE', #14521, 9.999999999999998224, 0.7853981633974561616 ) ;
#2660 = EDGE_CURVE ( 'NONE', #9451, #6871, #11535, .T. ) ;
#2661 = CARTESIAN_POINT ( 'NONE',  ( 193.8341126585712857, 7.327873325359597345, -16.70797078425209392 ) ) ;
#2662 = CARTESIAN_POINT ( 'NONE',  ( 208.6806335619233153, 11.77551824803669689, -26.30940818168328477 ) ) ;
#2663 = FACE_OUTER_BOUND ( 'NONE', #15843, .T. ) ;
#2664 = LINE ( 'NONE', #12320, #14185 ) ;
#2665 = CARTESIAN_POINT ( 'NONE',  ( 30.00000000000000355, 5.000000000000000000, -30.00000000000000000 ) ) ;
#2666 = CARTESIAN_POINT ( 'NONE',  ( 208.4761278624580711, 5.007259451653140125, -14.00000000000005507 ) ) ;
#2667 = VERTEX_POINT ( 'NONE', #404 ) ;
#2669 = EDGE_CURVE ( 'NONE', #4996, #13274, #3780, .T. ) ;
#2668 = CARTESIAN_POINT ( 'NONE',  ( 73.24173739811655537, 69.71069241403367300, -0.3690567165748998568 ) ) ;
#2670 = EDGE_LOOP ( 'NONE', ( #8116, #14442, #7233, #8193 ) ) ;
#2671 = AXIS2_PLACEMENT_3D ( 'NONE', #11043, #19405, #6249 ) ;
#2672 = ORIENTED_EDGE ( 'NONE', *, *, #3004, .T. ) ;
#2673 = CARTESIAN_POINT ( 'NONE',  ( 205.0662616026534693, 10.91332106064940888, -14.00000000000005507 ) ) ;
#2674 = DIRECTION ( 'NONE',  ( 0.8528685319524407227, 0.4924038765061096168, 0.1736481776669271115 ) ) ;
#2675 = EDGE_CURVE ( 'NONE', #4315, #5803, #710, .T. ) ;
#2676 =( GEOMETRIC_REPRESENTATION_CONTEXT ( 3 ) GLOBAL_UNCERTAINTY_ASSIGNED_CONTEXT ( ( #17640 ) ) GLOBAL_UNIT_ASSIGNED_CONTEXT ( ( #13415, #7036, #20186 ) ) REPRESENTATION_CONTEXT ( 'NONE', 'WORKASPACE' ) );
#2677 = CARTESIAN_POINT ( 'NONE',  ( 0.000000000000000000, 0.000000000000000000, 0.000000000000000000 ) ) ;
#2678 = DIRECTION ( 'NONE',  ( 0.000000000000000000, -6.938893903907167518E-18, -1.000000000000000000 ) ) ;
#2679 = EDGE_LOOP ( 'NONE', ( #12109, #14763, #15148, #3248, #16098, #14705, #10223, #8434, #14530, #18412 ) ) ;
#2680 = CARTESIAN_POINT ( 'NONE',  ( 211.7903592300262119, 6.147911733231966380, -2.561001429077395475 ) ) ;
#2681 = CARTESIAN_POINT ( 'NONE',  ( 201.4921241270915857, 0.4598221481815398803, -5.186396688528427390 ) ) ;
#2682 = FACE_BOUND ( 'NONE', #287, .T. ) ;
#2683 = CARTESIAN_POINT ( 'NONE',  ( 212.2669970461267042, 13.31505690926096364, -24.01557619556987788 ) ) ;
#2684 = EDGE_CURVE ( 'NONE', #3901, #12877, #16827, .T. ) ;
#2685 = EDGE_CURVE ( 'NONE', #12506, #19519, #47, .T. ) ;
#2686 = VECTOR ( 'NONE', #3066, 1000.000000000000114 ) ;
#2687 = CARTESIAN_POINT ( 'NONE',  ( 228.6857502674706950, 38.29359511746564948, -17.27917287590625151 ) ) ;
#2688 = CARTESIAN_POINT ( 'NONE',  ( -12.45686459883834196, 60.55839683866341261, -3.534893197518178987 ) ) ;
#2689 = CARTESIAN_POINT ( 'NONE',  ( 205.5965122587965084, 9.994899983462953941, -14.00000000000005507 ) ) ;
#2690 = CARTESIAN_POINT ( 'NONE',  ( 205.5965122587965084, 9.994899983462953941, -14.00000000000005507 ) ) ;
#2691 = CARTESIAN_POINT ( 'NONE',  ( -11.09026189855742572, 15.43276121221095920, 0.9457651797581775321 ) ) ;
#2692 = ORIENTED_EDGE ( 'NONE', *, *, #5085, .F. ) ;
#2694 = EDGE_CURVE ( 'NONE', #142, #5642, #2407, .T. ) ;
#2693 = CARTESIAN_POINT ( 'NONE',  ( 226.6211368133091923, 39.11482588413117867, -14.00000000000005507 ) ) ;
#2695 = DIRECTION ( 'NONE',  ( 1.000000000000000000, 0.000000000000000000, 0.000000000000000000 ) ) ;
#2696 = CARTESIAN_POINT ( 'NONE',  ( 220.8342687355452654, 32.21922912141519646, -15.81459191843844003 ) ) ;
#2697 = DIRECTION ( 'NONE',  ( -0.5000000000000027756, 0.8660254037844370423, -4.885182764539217401E-15 ) ) ;
#2699 = EDGE_LOOP ( 'NONE', ( #4873, #18756, #17160, #20529, #17770 ) ) ;
#2698 = ORIENTED_EDGE ( 'NONE', *, *, #1537, .F. ) ;
#2700 = VECTOR ( 'NONE', #20829, 1000.000000000000227 ) ;
#2701 = FACE_OUTER_BOUND ( 'NONE', #16340, .T. ) ;
#2702 = DIRECTION ( 'NONE',  ( 1.000000000000000000, 0.000000000000000000, 0.000000000000000000 ) ) ;
#2703 = ORIENTED_EDGE ( 'NONE', *, *, #12792, .F. ) ;
#2704 = EDGE_CURVE ( 'NONE', #17213, #11315, #15258, .T. ) ;
#2705 = CARTESIAN_POINT ( 'NONE',  ( 226.7180567368605182, 42.02820936217297998, -16.57782486433068669 ) ) ;
#2706 = FACE_OUTER_BOUND ( 'NONE', #10200, .T. ) ;
#2707 = B_SPLINE_CURVE_WITH_KNOTS ( 'NONE', 3,
 ( #18022, #4875, #9737, #3493 ),
 .UNSPECIFIED., .F., .F.,
 ( 4, 4 ),
 ( 2.946819598302503673E-07, 0.0008542804199448367306 ),
 .UNSPECIFIED. ) ;
#2708 = ORIENTED_EDGE ( 'NONE', *, *, #13170, .T. ) ;
#2709 = CARTESIAN_POINT ( 'NONE',  ( -34.00000000000000711, 65.74999999999997158, 2.481238266578629226 ) ) ;
#2710 = VERTEX_POINT ( 'NONE', #7167 ) ;
#2711 = CARTESIAN_POINT ( 'NONE',  ( 10.49211908931699178, 0.000000000000000000, 0.000000000000000000 ) ) ;
#2712 = DIRECTION ( 'NONE',  ( 0.000000000000000000, 0.000000000000000000, 1.000000000000000000 ) ) ;
#2713 = VECTOR ( 'NONE', #15106, 1000.000000000000114 ) ;
#2714 = VERTEX_POINT ( 'NONE', #13652 ) ;
#2715 = CARTESIAN_POINT ( 'NONE',  ( 199.9261466397861113, -0.4442953756591617176, -7.343163769975552313 ) ) ;
#2716 = FACE_OUTER_BOUND ( 'NONE', #2577, .T. ) ;
#2717 = DIRECTION ( 'NONE',  ( 0.000000000000000000, -0.7775157341893068619, -0.6288634852557930532 ) ) ;
#2718 = LINE ( 'NONE', #18403, #770 ) ;
#2719 = CARTESIAN_POINT ( 'NONE',  ( 215.9094043865061110, 15.77204112533624958, -11.19512133156266032 ) ) ;
#2720 = VERTEX_POINT ( 'NONE', #6853 ) ;
#2721 = ORIENTED_EDGE ( 'NONE', *, *, #14023, .T. ) ;
#2722 = LINE ( 'NONE', #9162, #5113 ) ;
#2723 = EDGE_LOOP ( 'NONE', ( #19092, #6082, #335, #2194, #8230, #7344 ) ) ;
#2724 = EDGE_LOOP ( 'NONE', ( #9285, #1905 ) ) ;
#2725 = VERTEX_POINT ( 'NONE', #13546 ) ;
#2726 = CARTESIAN_POINT ( 'NONE',  ( -17.30948708500259414, 10.26275758369035529, 12.43542173818663699 ) ) ;
#2727 = CARTESIAN_POINT ( 'NONE',  ( 226.8653541683588628, 40.79361683593005949, -10.33191597617938484 ) ) ;
#2728 = DIRECTION ( 'NONE',  ( 0.000000000000000000, -0.5000000000000009992, -0.8660254037844380415 ) ) ;
#2729 = LINE ( 'NONE', #17243, #19805 ) ;
#2730 = CARTESIAN_POINT ( 'NONE',  ( 5.000000000000000000, 0.000000000000000000, 0.000000000000000000 ) ) ;
#2731 = AXIS2_PLACEMENT_3D ( 'NONE', #11154, #7964, #1104 ) ;
#2732 = ORIENTED_EDGE ( 'NONE', *, *, #16416, .F. ) ;
#2733 = DIRECTION ( 'NONE',  ( 0.5000000000000015543, -0.8660254037844377084, 0.000000000000000000 ) ) ;
#2734 = CIRCLE ( 'NONE', #13920, 5.999999999999989342 ) ;
#2735 = DIRECTION ( 'NONE',  ( 0.8660254037844369313, 0.5000000000000029976, 4.996003610813203446E-16 ) ) ;
#2736 = CARTESIAN_POINT ( 'NONE',  ( -18.73438247807179380, 45.53180543536074509, -12.20217720735596068 ) ) ;
#2737 = CARTESIAN_POINT ( 'NONE',  ( 209.0908153953612612, 5.362149464242316199, -1.545471579934816875 ) ) ;
#2738 = LINE ( 'NONE', #5895, #8445 ) ;
#2739 = CARTESIAN_POINT ( 'NONE',  ( -28.50078905930214290, 49.62758644748794978, 0.2159913647941864856 ) ) ;
#2740 = EDGE_CURVE ( 'NONE', #1834, #9609, #5251, .T. ) ;
#2742 = ORIENTED_EDGE ( 'NONE', *, *, #20819, .F. ) ;
#2741 = ORIENTED_EDGE ( 'NONE', *, *, #13033, .F. ) ;
#2743 = VECTOR ( 'NONE', #14626, 1000.000000000000227 ) ;
#2744 = DIRECTION ( 'NONE',  ( 0.5000000000000046629, -0.8660254037844359321, 0.000000000000000000 ) ) ;
#2745 = CARTESIAN_POINT ( 'NONE',  ( 208.8026598822967514, 11.49194359559607115, -2.204078039983189630 ) ) ;
#2746 = CARTESIAN_POINT ( 'NONE',  ( -2.766997014963338053, 76.74099499729231866, -3.129240771527075804 ) ) ;
#2747 = VECTOR ( 'NONE', #1310, 1000.000000000000000 ) ;
#2748 = VERTEX_POINT ( 'NONE', #11956 ) ;
#2749 = VERTEX_POINT ( 'NONE', #19998 ) ;
#2750 = PLANE ( 'NONE',  #10189 ) ;
#2751 = FACE_OUTER_BOUND ( 'NONE', #8635, .T. ) ;
#2752 = CARTESIAN_POINT ( 'NONE',  ( -7.585160902965351504, 50.15125659263410540, -14.64997619612770485 ) ) ;
#2753 = CARTESIAN_POINT ( 'NONE',  ( -26.41341864416630969, 9.999999999999992895, -6.948775141111584119 ) ) ;
#2754 = VERTEX_POINT ( 'NONE', #16510 ) ;
#2755 = EDGE_LOOP ( 'NONE', ( #15288, #4387, #20400, #14266 ) ) ;
#2756 = CARTESIAN_POINT ( 'NONE',  ( 0.4195860999641303213, 70.63162242946638969, 1.437809060325977661 ) ) ;
#2757 = TOROIDAL_SURFACE ( 'NONE', #11894, 0.9999999999999974465, 1.500000000000000000 ) ;
#2759 = ADVANCED_FACE ( 'NONE', ( #10442 ), #8864, .F. ) ;
#2758 = CARTESIAN_POINT ( 'NONE',  ( 10.49211908931699178, 0.000000000000000000, 5.999999999999998224 ) ) ;
#2760 = AXIS2_PLACEMENT_3D ( 'NONE', #8227, #19377, #17790 ) ;
#2761 = DIRECTION ( 'NONE',  ( 0.5000000000000039968, -0.8660254037844362651, 0.000000000000000000 ) ) ;
#2762 = CARTESIAN_POINT ( 'NONE',  ( 216.6299025733443102, 15.83398158984899240, -14.00000000000005507 ) ) ;
#2763 = VECTOR ( 'NONE', #9883, 1000.000000000000114 ) ;
#2764 = LINE ( 'NONE', #7830, #19032 ) ;
#2765 = FACE_OUTER_BOUND ( 'NONE', #815, .T. ) ;
#2766 = DIRECTION ( 'NONE',  ( 0.5000000000000045519, -0.8660254037844360431, 1.445602896647343354E-16 ) ) ;
#2767 = EDGE_CURVE ( 'NONE', #3911, #15566, #15156, .T. ) ;
#2768 = ORIENTED_EDGE ( 'NONE', *, *, #7687, .T. ) ;
#2769 = CARTESIAN_POINT ( 'NONE',  ( -31.85380967428733712, 66.50634452888658643, 2.432944671160833572 ) ) ;
#2770 = CARTESIAN_POINT ( 'NONE',  ( 208.5625094892126583, 11.70731928285941770, -25.48492467622476099 ) ) ;
#2771 = DIRECTION ( 'NONE',  ( 1.000000000000000000, 0.000000000000000000, 0.000000000000000000 ) ) ;
#2772 = ADVANCED_FACE ( 'NONE', ( #10120 ), #2305, .T. ) ;
#2773 = VERTEX_POINT ( 'NONE', #6735 ) ;
#2774 = CARTESIAN_POINT ( 'NONE',  ( 81.47405289336727208, 65.45330303017013307, 0.4987988714753746611 ) ) ;
#2775 = VECTOR ( 'NONE', #1213, 1000.000000000000114 ) ;
#2776 = ORIENTED_EDGE ( 'NONE', *, *, #4882, .F. ) ;
#2777 = ORIENTED_EDGE ( 'NONE', *, *, #7465, .F. ) ;
#2778 = CARTESIAN_POINT ( 'NONE',  ( -2.450339071221972365, 64.25000000000000000, 3.021668726329232779 ) ) ;
#2779 = VECTOR ( 'NONE', #3257, 1000.000000000000227 ) ;
#2780 = VECTOR ( 'NONE', #15502, 1000.000000000000227 ) ;
#2781 = PRODUCT_CONTEXT ( 'NONE', #12849, 'mechanical' ) ;
#2782 = CARTESIAN_POINT ( 'NONE',  ( 199.4915863999364660, 6.470219395467344370, -4.494676796018650222 ) ) ;
#2783 = EDGE_LOOP ( 'NONE', ( #11949, #13867, #12411, #8559 ) ) ;
#2784 = DIRECTION ( 'NONE',  ( 0.000000000000000000, 0.000000000000000000, -1.000000000000000000 ) ) ;
#2785 = CARTESIAN_POINT ( 'NONE',  ( 0.3999999999999975797, 0.000000000000000000, 6.500000000000000000 ) ) ;
#2786 = DIRECTION ( 'NONE',  ( -0.000000000000000000, -1.000000000000000000, -0.000000000000000000 ) ) ;
#2787 = DIRECTION ( 'NONE',  ( -0.5000000000000049960, 0.8660254037844357100, -0.000000000000000000 ) ) ;
#2788 = EDGE_CURVE ( 'NONE', #3973, #3166, #1990, .T. ) ;
#2789 = ORIENTED_EDGE ( 'NONE', *, *, #4236, .F. ) ;
#2790 = CARTESIAN_POINT ( 'NONE',  ( 4.000000000000000000, 0.000000000000000000, 0.000000000000000000 ) ) ;
#2791 = CONICAL_SURFACE ( 'NONE', #9200, 4.509097725792825528, 0.5235987755983015912 ) ;
#2792 = ADVANCED_FACE ( 'NONE', ( #7368 ), #12568, .T. ) ;
#2793 = AXIS2_PLACEMENT_3D ( 'NONE', #10566, #15166, #13557 ) ;
#2794 = DIRECTION ( 'NONE',  ( -0.7559289460184535070, 0.000000000000000000, -0.6546536707079781969 ) ) ;
#2795 = LINE ( 'NONE', #9233, #12230 ) ;
#2796 = FACE_OUTER_BOUND ( 'NONE', #12081, .T. ) ;
#2797 = ORIENTED_EDGE ( 'NONE', *, *, #17468, .F. ) ;
#2798 = DIRECTION ( 'NONE',  ( 0.5000000000000055511, -0.8660254037844353769, -3.885780586188047891E-16 ) ) ;
#2799 = EDGE_CURVE ( 'NONE', #15099, #16403, #15910, .T. ) ;
#2800 = CARTESIAN_POINT ( 'NONE',  ( 4.000000000000000000, 1.759474945355379960, -3.047500000000001652 ) ) ;
#2801 = ADVANCED_FACE ( 'NONE', ( #13974 ), #12275, .T. ) ;
#2802 = FACE_OUTER_BOUND ( 'NONE', #6364, .T. ) ;
#2803 = CARTESIAN_POINT ( 'NONE',  ( -33.32035108112687993, 77.22491497699215302, -3.799191488838269848 ) ) ;
#2804 = EDGE_CURVE ( 'NONE', #9345, #7191, #6784, .T. ) ;
#2806 = EDGE_LOOP ( 'NONE', ( #11116, #1546, #14669, #20944 ) ) ;
#2805 = VERTEX_POINT ( 'NONE', #15568 ) ;
#2807 = EDGE_CURVE ( 'NONE', #4238, #13744, #12584, .T. ) ;
#2808 = CARTESIAN_POINT ( 'NONE',  ( -11.00000000000000355, 15.09941697557068530, 11.45643923738960446 ) ) ;
#2809 =( NAMED_UNIT ( * ) PLANE_ANGLE_UNIT ( ) SI_UNIT ( $, .RADIAN. ) );
#2810 = ORIENTED_EDGE ( 'NONE', *, *, #1533, .F. ) ;
#2811 = VECTOR ( 'NONE', #20786, 1000.000000000000114 ) ;
#2812 = VECTOR ( 'NONE', #6394, 1000.000000000000114 ) ;
#2813 = CARTESIAN_POINT ( 'NONE',  ( -46.99999999999998579, 64.25000000000000000, -2.528164662410438357 ) ) ;
#2814 = DIRECTION ( 'NONE',  ( -0.5000000000000045519, 0.8660254037844361541, 0.000000000000000000 ) ) ;
#2815 = PLANE ( 'NONE',  #161 ) ;
#2816 = EDGE_CURVE ( 'NONE', #20850, #14308, #9590, .T. ) ;
#2817 = LINE ( 'NONE', #17224, #20375 ) ;
#2818 = ORIENTED_EDGE ( 'NONE', *, *, #19616, .T. ) ;
#2819 = DIRECTION ( 'NONE',  ( 0.8660254037844370423, 0.5000000000000027756, 0.000000000000000000 ) ) ;
#2820 = FACE_OUTER_BOUND ( 'NONE', #8759, .T. ) ;
#2821 = EDGE_CURVE ( 'NONE', #10684, #11395, #8310, .T. ) ;
#2822 = AXIS2_PLACEMENT_3D ( 'NONE', #18744, #18535, #11968 ) ;
#2823 = FACE_OUTER_BOUND ( 'NONE', #18288, .T. ) ;
#2824 = DIRECTION ( 'NONE',  ( -0.8660254037844380415, -0.5000000000000008882, 0.000000000000000000 ) ) ;
#2825 = EDGE_LOOP ( 'NONE', ( #17109, #5775, #16417, #8921 ) ) ;
#2826 = ORIENTED_EDGE ( 'NONE', *, *, #9701, .T. ) ;
#2827 = CARTESIAN_POINT ( 'NONE',  ( 199.2144802262915846, 21.04890371929339921, -14.00000000000005507 ) ) ;
#2828 = EDGE_CURVE ( 'NONE', #11210, #9561, #10761, .T. ) ;
#2829 = EDGE_LOOP ( 'NONE', ( #17064, #1727, #12572, #7279, #20224, #20917 ) ) ;
#2830 = EDGE_CURVE ( 'NONE', #8298, #11548, #12930, .T. ) ;
#2831 = CARTESIAN_POINT ( 'NONE',  ( -17.62346795288569368, 10.35879774359155903, 12.39796379449725805 ) ) ;
#2832 = CARTESIAN_POINT ( 'NONE',  ( 80.63605647399829479, 53.05720336860252928, -4.117601259720633955 ) ) ;
#2833 = PLANE ( 'NONE',  #2938 ) ;
#2834 = EDGE_CURVE ( 'NONE', #5980, #2640, #7266, .T. ) ;
#2835 = CARTESIAN_POINT ( 'NONE',  ( 229.7218892158732615, 36.82541889109744204, -14.53509620734055829 ) ) ;
#2836 = VECTOR ( 'NONE', #7046, 1000.000000000000227 ) ;
#2837 = EDGE_CURVE ( 'NONE', #3359, #10810, #9269, .T. ) ;
#2838 = ORIENTED_EDGE ( 'NONE', *, *, #2843, .F. ) ;
#2839 = DIRECTION ( 'NONE',  ( 0.8660254037844352659, 0.5000000000000056621, 0.000000000000000000 ) ) ;
#2840 = CARTESIAN_POINT ( 'NONE',  ( 211.7903592300262119, 6.147911733231966380, -2.561001429077395475 ) ) ;
#2841 = CARTESIAN_POINT ( 'NONE',  ( -17.38132050553625518, 45.61375688610377921, -12.44240297365142567 ) ) ;
#2842 = CARTESIAN_POINT ( 'NONE',  ( 228.8533067253947877, 37.35038200410757270, -11.12998660979008392 ) ) ;
#2843 = EDGE_CURVE ( 'NONE', #3717, #5485, #15465, .T. ) ;
#2844 = CARTESIAN_POINT ( 'NONE',  ( 226.6139186294880119, 42.20858185514595107, -16.83383072344315678 ) ) ;
#2845 = DIRECTION ( 'NONE',  ( 0.000000000000000000, 0.000000000000000000, 1.000000000000000000 ) ) ;
#2847 = ORIENTED_EDGE ( 'NONE', *, *, #17548, .F. ) ;
#2846 = ORIENTED_EDGE ( 'NONE', *, *, #16678, .T. ) ;
#2848 = EDGE_LOOP ( 'NONE', ( #9137, #10756, #20123 ) ) ;
#2849 = VECTOR ( 'NONE', #20466, 1000.000000000000114 ) ;
#2850 = DIRECTION ( 'NONE',  ( -0.000000000000000000, -0.000000000000000000, 1.000000000000000000 ) ) ;
#2851 = APPLICATION_CONTEXT ( 'automotive_design' ) ;
#2852 = CIRCLE ( 'NONE', #9254, 12.47473710546057823 ) ;
#2853 = DIRECTION ( 'NONE',  ( -0.5000000000000054401, 0.8660254037844354880, -0.000000000000000000 ) ) ;
#2854 = ORIENTED_EDGE ( 'NONE', *, *, #843, .T. ) ;
#2855 = ORIENTED_EDGE ( 'NONE', *, *, #15536, .T. ) ;
#2856 = CARTESIAN_POINT ( 'NONE',  ( 30.00000000000000355, 0.000000000000000000, -15.00000000000000000 ) ) ;
#2857 = CARTESIAN_POINT ( 'NONE',  ( -31.74999999999995737, 9.242062880866318385E-16, -8.000000000000058620 ) ) ;
#2858 = CARTESIAN_POINT ( 'NONE',  ( 0.9502985271742134810, 56.92418902563075278, 0.1464156901064357363 ) ) ;
#2859 = DIRECTION ( 'NONE',  ( 0.000000000000000000, 0.000000000000000000, 1.000000000000000000 ) ) ;
#2860 = VERTEX_POINT ( 'NONE', #10871 ) ;
#2861 = VERTEX_POINT ( 'NONE', #15771 ) ;
#2862 = FACE_OUTER_BOUND ( 'NONE', #18703, .T. ) ;
#2863 = CARTESIAN_POINT ( 'NONE',  ( 207.3946896431964149, 11.03307818039693267, -25.65046807331635392 ) ) ;
#2864 = LINE ( 'NONE', #9299, #16071 ) ;
#2865 = EDGE_CURVE ( 'NONE', #9778, #3962, #3769, .T. ) ;
#2866 = LINE ( 'NONE', #19081, #20280 ) ;
#2867 = CARTESIAN_POINT ( 'NONE',  ( 74.06428810979899424, 71.22525070374874190, -24.03620132832545764 ) ) ;
#2868 = DIRECTION ( 'NONE',  ( 0.6299240516454520655, 0.3636868207865263658, -0.6862416378687372642 ) ) ;
#2869 = CARTESIAN_POINT ( 'NONE',  ( -28.35076132082143374, 77.92717739396516663, 2.017250382391173158 ) ) ;
#2870 = CARTESIAN_POINT ( 'NONE',  ( -20.74071588547708700, 16.72200274001069431, 11.56693563242971123 ) ) ;
#2871 = DIRECTION ( 'NONE',  ( 0.000000000000000000, -1.000000000000000000, 1.232415585510385534E-15 ) ) ;
#2872 = FACE_OUTER_BOUND ( 'NONE', #8945, .T. ) ;
#2873 = DIRECTION ( 'NONE',  ( -0.000000000000000000, -1.000000000000000000, -0.000000000000000000 ) ) ;
#2874 = ORIENTED_EDGE ( 'NONE', *, *, #12114, .T. ) ;
#2875 = AXIS2_PLACEMENT_3D ( 'NONE', #20016, #20118, #18639 ) ;
#2876 = CARTESIAN_POINT ( 'NONE',  ( 73.00847438502604803, 74.24912532398991516, -0.7262419208828606587 ) ) ;
#2877 = ADVANCED_FACE ( 'NONE', ( #13863 ), #4099, .T. ) ;
#2878 = VERTEX_POINT ( 'NONE', #19440 ) ;
#2879 = ORIENTED_EDGE ( 'NONE', *, *, #16930, .T. ) ;
#2880 = CARTESIAN_POINT ( 'NONE',  ( -3.050656336052146589, 73.64887869708235257, -0.2211343278613356611 ) ) ;
#2881 = CARTESIAN_POINT ( 'NONE',  ( 5.000000000000004441, -3.513898075855354630, 2.028750000000002274 ) ) ;
#2882 = PRODUCT_CONTEXT ( 'NONE', #18541, 'mechanical' ) ;
#2883 = CARTESIAN_POINT ( 'NONE',  ( 9.999999999999998224, 6.987792986206746511E-16, 5.400000000000040323 ) ) ;
#2884 = ORIENTED_EDGE ( 'NONE', *, *, #15899, .F. ) ;
#2885 = CARTESIAN_POINT ( 'NONE',  ( 202.4269704670640238, 0.9995559342156025151, -23.72013913782470595 ) ) ;
#2886 = ADVANCED_FACE ( 'NONE', ( #20823 ), #7893, .F. ) ;
#2887 = DIRECTION ( 'NONE',  ( -0.8660254037844362651, -0.5000000000000045519, 5.976026924694053325E-17 ) ) ;
#2888 = CARTESIAN_POINT ( 'NONE',  ( 209.4688803963327928, 30.49173192974595992, -16.24689738482229728 ) ) ;
#2889 = CARTESIAN_POINT ( 'NONE',  ( 227.8547393642149927, 40.05941729951386066, -17.61401795338996124 ) ) ;
#2890 = EDGE_LOOP ( 'NONE', ( #656, #6702, #11561, #1980, #5146 ) ) ;
#2891 = LINE ( 'NONE', #17413, #15460 ) ;
#2892 = CARTESIAN_POINT ( 'NONE',  ( 202.6969606483661721, 7.966816499295318543, -2.204078039983093706 ) ) ;
#2893 = DIRECTION ( 'NONE',  ( 0.5000000000000044409, -0.8660254037844360431, 0.000000000000000000 ) ) ;
#2894 = PLANE ( 'NONE',  #5779 ) ;
#2895 = AXIS2_PLACEMENT_3D ( 'NONE', #6507, #9411, #1278 ) ;
#2896 = FACE_OUTER_BOUND ( 'NONE', #7470, .T. ) ;
#2897 = ORIENTED_EDGE ( 'NONE', *, *, #15349, .F. ) ;
#2898 = CARTESIAN_POINT ( 'NONE',  ( 194.6438684810882194, 7.795386067467640068, -19.29168348739290550 ) ) ;
#2899 = CARTESIAN_POINT ( 'NONE',  ( -4.618023652948263447, 68.30950415664239017, 5.167706431871527784 ) ) ;
#2900 = DIRECTION ( 'NONE',  ( 0.000000000000000000, 6.938893903907178303E-18, 1.000000000000000000 ) ) ;
#2901 = DIRECTION ( 'NONE',  ( -0.8660254037844357100, -0.5000000000000051070, 0.000000000000000000 ) ) ;
#2902 = FACE_OUTER_BOUND ( 'NONE', #938, .T. ) ;
#2904 = EDGE_LOOP ( 'NONE', ( #10747, #1361, #2579, #19863, #12319, #1498 ) ) ;
#2903 = VERTEX_POINT ( 'NONE', #12893 ) ;
#2905 = CARTESIAN_POINT ( 'NONE',  ( 227.9553588074475670, 39.88513931160575510, -14.00000000000005507 ) ) ;
#2906 = CARTESIAN_POINT ( 'NONE',  ( 22.32500173739930460, 255.2883321626825932, 8.042028396309257587 ) ) ;
#2907 = ORIENTED_EDGE ( 'NONE', *, *, #8738, .T. ) ;
#2908 = ADVANCED_FACE ( 'NONE', ( #11496 ), #13101, .T. ) ;
#2909 = DIRECTION ( 'NONE',  ( 0.5000000000000046629, -0.8660254037844360431, 0.000000000000000000 ) ) ;
#2910 = EDGE_LOOP ( 'NONE', ( #13458, #9217, #12056, #15316 ) ) ;
#2911 = CONICAL_SURFACE ( 'NONE', #7961, 10.85470691220533190, 0.8171114040043576665 ) ;
#2912 = ADVANCED_FACE ( 'NONE', ( #3439 ), #11552, .F. ) ;
#2913 = CIRCLE ( 'NONE', #8303, 12.47473710546057823 ) ;
#2914 = DIRECTION ( 'NONE',  ( 0.5000000000000051070, -0.8660254037844359321, 0.000000000000000000 ) ) ;
#2915 = ORIENTED_EDGE ( 'NONE', *, *, #18518, .T. ) ;
#2916 = CARTESIAN_POINT ( 'NONE',  ( -15.99999999999999289, 15.09941697557068530, 0.9999999999999991118 ) ) ;
#2917 = EDGE_CURVE ( 'NONE', #9370, #2041, #1340, .T. ) ;
#2918 = EDGE_LOOP ( 'NONE', ( #509, #20075, #113, #10552 ) ) ;
#2919 = CARTESIAN_POINT ( 'NONE',  ( 200.0157312721003393, 23.75418783301503112, -14.00000000000005507 ) ) ;
#2920 = CARTESIAN_POINT ( 'NONE',  ( 0.000000000000000000, 0.000000000000000000, 0.000000000000000000 ) ) ;
#2921 = AXIS2_PLACEMENT_3D ( 'NONE', #15678, #12586, #19148 ) ;
#2922 = CARTESIAN_POINT ( 'NONE',  ( 209.8577037357181894, 2.614299844655262106, -14.00000000000005507 ) ) ;
#2923 = CARTESIAN_POINT ( 'NONE',  ( 62.36389338619030553, 105.9389375482328006, -12.50000000000000000 ) ) ;
#2924 = VECTOR ( 'NONE', #8682, 1000.000000000000114 ) ;
#2925 = VERTEX_POINT ( 'NONE', #15979 ) ;
#2926 = VECTOR ( 'NONE', #625, 1000.000000000000000 ) ;
#2927 = CARTESIAN_POINT ( 'NONE',  ( 217.4948448325154970, 10.21421812206089541, -7.132002368301439077 ) ) ;
#2928 = EDGE_CURVE ( 'NONE', #2748, #10227, #18337, .T. ) ;
#2929 = VERTEX_POINT ( 'NONE', #7995 ) ;
#2930 = DIRECTION ( 'NONE',  ( -0.8660254037844355990, -0.5000000000000055511, 0.000000000000000000 ) ) ;
#2931 = CARTESIAN_POINT ( 'NONE',  ( 207.6064227804952225, 10.80129578285631453, -1.876704962899016893 ) ) ;
#2932 = CARTESIAN_POINT ( 'NONE',  ( 209.5209968812125112, 4.837694770255529519, -27.13030671846411579 ) ) ;
#2933 = EDGE_CURVE ( 'NONE', #12370, #15417, #20357, .T. ) ;
#2934 = CARTESIAN_POINT ( 'NONE',  ( 226.6211368133091923, 39.11482588413117867, -14.00000000000005507 ) ) ;
#2935 = DIRECTION ( 'NONE',  ( 0.000000000000000000, 0.000000000000000000, 1.000000000000000000 ) ) ;
#2936 = CIRCLE ( 'NONE', #20190, 4.999999999999997335 ) ;
#2937 = ORIENTED_EDGE ( 'NONE', *, *, #263, .T. ) ;
#2938 = AXIS2_PLACEMENT_3D ( 'NONE', #14077, #5985, #20825 ) ;
#2939 = CARTESIAN_POINT ( 'NONE',  ( 215.8574505745143597, 8.496048015791016539, -5.407152407594054466 ) ) ;
#2940 = EDGE_CURVE ( 'NONE', #16536, #8857, #10071, .T. ) ;
#2941 = EDGE_CURVE ( 'NONE', #9185, #6444, #10528, .T. ) ;
#2942 =( LENGTH_UNIT ( ) NAMED_UNIT ( * ) SI_UNIT ( .MILLI., .METRE. ) );
#2943 = CARTESIAN_POINT ( 'NONE',  ( -4.380992799470656784, 51.87686864743692894, -5.137587943657599077 ) ) ;
#2944 = CARTESIAN_POINT ( 'NONE',  ( 210.2598317367304332, 3.924419927273977482, -14.00000000000005507 ) ) ;
#2945 = DIRECTION ( 'NONE',  ( -1.000000000000000000, 0.000000000000000000, 0.000000000000000000 ) ) ;
#2946 = CARTESIAN_POINT ( 'NONE',  ( -27.35016751773910570, 45.66839489749002468, -5.250096803208007756 ) ) ;
#2948 = ORIENTED_EDGE ( 'NONE', *, *, #20162, .T. ) ;
#2947 = ORIENTED_EDGE ( 'NONE', *, *, #9251, .F. ) ;
#2949 = VERTEX_POINT ( 'NONE', #17764 ) ;
#2950 = DIRECTION ( 'NONE',  ( -1.000000000000000000, 0.000000000000000000, -0.000000000000000000 ) ) ;
#2951 = CARTESIAN_POINT ( 'NONE',  ( 226.1897974575875310, 41.96371538238017251, -16.83383072344315678 ) ) ;
#2952 = EDGE_CURVE ( 'NONE', #17941, #6800, #12690, .T. ) ;
#2953 = CARTESIAN_POINT ( 'NONE',  ( 229.7396837492933344, 36.79459785511654957, -15.57898118447804769 ) ) ;
#2954 = ORIENTED_EDGE ( 'NONE', *, *, #13976, .T. ) ;
#2955 = AXIS2_PLACEMENT_3D ( 'NONE', #19299, #7847, #1497 ) ;
#2956 = CARTESIAN_POINT ( 'NONE',  ( 218.8515590432435260, 37.13686462750394668, -16.82415462623104574 ) ) ;
#2957 = CARTESIAN_POINT ( 'NONE',  ( 229.5092485165274070, 36.86725431015519661, -15.51567023025828718 ) ) ;
#2958 = CARTESIAN_POINT ( 'NONE',  ( -14.44414019777457092, 50.46616997920651215, -16.21138906647247779 ) ) ;
#2959 = DIRECTION ( 'NONE',  ( -0.000000000000000000, 0.8660254037844394848, 0.4999999999999985012 ) ) ;
#2960 = VERTEX_POINT ( 'NONE', #19250 ) ;
#2961 = ORIENTED_EDGE ( 'NONE', *, *, #1563, .T. ) ;
#2962 = CARTESIAN_POINT ( 'NONE',  ( 219.5770999726424861, 36.52806405021930658, -17.68583624946726474 ) ) ;
#2963 = EDGE_CURVE ( 'NONE', #15695, #5066, #6124, .T. ) ;
#2964 = DIRECTION ( 'NONE',  ( 0.5000000000000044409, -0.8660254037844360431, -0.000000000000000000 ) ) ;
#2965 = B_SPLINE_CURVE_WITH_KNOTS ( 'NONE', 3,
 ( #19781, #5562, #15152, #8755 ),
 .UNSPECIFIED., .F., .F.,
 ( 4, 4 ),
 ( 4.196882779819118193E-05, 0.0006078950500808810720 ),
 .UNSPECIFIED. ) ;
#2966 = DIRECTION ( 'NONE',  ( -0.5000000000000058842, 0.8660254037844351549, 0.000000000000000000 ) ) ;
#2967 = DIRECTION ( 'NONE',  ( 0.000000000000000000, 0.000000000000000000, 1.000000000000000000 ) ) ;
#2968 = AXIS2_PLACEMENT_3D ( 'NONE', #6122, #15803, #9405 ) ;
#2969 = CARTESIAN_POINT ( 'NONE',  ( 205.0443405901917231, 9.676103521955074172, -13.34105989163307981 ) ) ;
#2970 = CARTESIAN_POINT ( 'NONE',  ( 221.4106920200644026, 33.14621139776020442, -11.20506451332633446 ) ) ;
#2971 = DIRECTION ( 'NONE',  ( -0.4758887346169484722, -0.2747544890354094993, -0.8354878114129318245 ) ) ;
#2972 = APPLICATION_CONTEXT ( 'automotive_design' ) ;
#2973 = ORIENTED_EDGE ( 'NONE', *, *, #7030, .F. ) ;
#2974 = AXIS2_PLACEMENT_3D ( 'NONE', #4193, #1015, #15557 ) ;
#2975 = DIRECTION ( 'NONE',  ( 0.8660254037844352659, 0.5000000000000056621, 0.000000000000000000 ) ) ;
#2976 = DIRECTION ( 'NONE',  ( -0.5000000000000008882, 0.8660254037844381525, 0.000000000000000000 ) ) ;
#2977 = CARTESIAN_POINT ( 'NONE',  ( 220.3453756550692617, 33.06601677626848357, -11.10922658182128941 ) ) ;
#2978 = VERTEX_POINT ( 'NONE', #17559 ) ;
#2979 = CARTESIAN_POINT ( 'NONE',  ( 71.09010947823266235, 73.07777849309526630, -2.093657812535054674 ) ) ;
#2980 = ORIENTED_EDGE ( 'NONE', *, *, #13365, .T. ) ;
#2981 = ORIENTED_EDGE ( 'NONE', *, *, #19238, .T. ) ;
#2982 = DIRECTION ( 'NONE',  ( 0.8660254037844370423, 0.5000000000000026645, -0.000000000000000000 ) ) ;
#2983 = CARTESIAN_POINT ( 'NONE',  ( 200.9720064151970575, -0.09806717659808367182, -6.376588578941771779 ) ) ;
#2984 = B_SPLINE_CURVE_WITH_KNOTS ( 'NONE', 3,
 ( #9379, #15874, #9483, #14715 ),
 .UNSPECIFIED., .F., .F.,
 ( 4, 4 ),
 ( 0.009226128036593859993, 0.009807580604158035870 ),
 .UNSPECIFIED. ) ;
#2985 = AXIS2_PLACEMENT_3D ( 'NONE', #15650, #1117, #1323 ) ;
#2986 = B_SPLINE_CURVE_WITH_KNOTS ( 'NONE', 3,
 ( #11356, #17832, #9748, #16235 ),
 .UNSPECIFIED., .F., .F.,
 ( 4, 4 ),
 ( 2.986363092411206710E-07, 0.0004523518780891170763 ),
 .UNSPECIFIED. ) ;
#2987 = DIRECTION ( 'NONE',  ( -0.8426815769442658199, -0.4865224352899169546, 0.2306158707424407761 ) ) ;
#2988 = APPLICATION_PROTOCOL_DEFINITION ( 'draft international standard', 'automotive_design', 1998, #4458 ) ;
#2989 = AXIS2_PLACEMENT_3D ( 'NONE', #4273, #20167, #12019 ) ;
#2990 = CARTESIAN_POINT ( 'NONE',  ( 219.3291089353582493, 36.33974875727300002, -10.64970491435233058 ) ) ;
#2991 = ORIENTED_EDGE ( 'NONE', *, *, #15456, .F. ) ;
#2992 = DIRECTION ( 'NONE',  ( 0.000000000000000000, -1.000000000000000000, 0.000000000000000000 ) ) ;
#2993 = CARTESIAN_POINT ( 'NONE',  ( 60.60228022274862525, 122.9901410505958523, 41.00000000000001421 ) ) ;
#2994 = DIRECTION ( 'NONE',  ( 0.000000000000000000, -0.5000000000000009992, -0.8660254037844380415 ) ) ;
#2995 = DIRECTION ( 'NONE',  ( 0.5000000000000045519, -0.8660254037844360431, 0.000000000000000000 ) ) ;
#2996 = DIRECTION ( 'NONE',  ( -0.8660254037844354880, -0.5000000000000055511, 0.000000000000000000 ) ) ;
#2997 = DIRECTION ( 'NONE',  ( 0.8660254037844380415, 0.5000000000000014433, 0.000000000000000000 ) ) ;
#2998 = CARTESIAN_POINT ( 'NONE',  ( 200.7657312721003393, 22.45514972733838022, -14.00000000000005507 ) ) ;
#2999 = LINE ( 'NONE', #9440, #4450 ) ;
#3000 = LINE ( 'NONE', #20583, #267 ) ;
#3001 = ORIENTED_EDGE ( 'NONE', *, *, #17168, .T. ) ;
#3002 = CARTESIAN_POINT ( 'NONE',  ( 127.2868417743716094, 73.48909236273162549, -7.887051853916060842E-15 ) ) ;
#3003 = CARTESIAN_POINT ( 'NONE',  ( 58.57586221349259858, 85.50000000000002842, -12.50000000002017231 ) ) ;
#3004 = EDGE_CURVE ( 'NONE', #10783, #3306, #3030, .T. ) ;
#3005 = LINE ( 'NONE', #1519, #7771 ) ;
#3007 = ORIENTED_EDGE ( 'NONE', *, *, #16163, .F. ) ;
#3006 = EDGE_LOOP ( 'NONE', ( #12160, #6518, #16180, #7602 ) ) ;
#3008 = DIRECTION ( 'NONE',  ( 0.000000000000000000, -1.000000000000000000, 0.000000000000000000 ) ) ;
#3009 = CARTESIAN_POINT ( 'NONE',  ( 43.00000000000000000, 0.000000000000000000, 0.000000000000000000 ) ) ;
#3010 = AXIS2_PLACEMENT_3D ( 'NONE', #11273, #4494, #1622 ) ;
#3011 = ORIENTED_EDGE ( 'NONE', *, *, #18559, .T. ) ;
#3012 = CARTESIAN_POINT ( 'NONE',  ( 218.2982806543416530, 38.53706601724700676, -14.99046307270422318 ) ) ;
#3013 = DIRECTION ( 'NONE',  ( -0.5000000000000054401, 0.8660254037844354880, -0.000000000000000000 ) ) ;
#3014 = ORIENTED_EDGE ( 'NONE', *, *, #8516, .T. ) ;
#3015 = AXIS2_PLACEMENT_3D ( 'NONE', #16984, #2355, #13703 ) ;
#3016 = ADVANCED_FACE ( 'NONE', ( #5021, #3339 ), #16182, .T. ) ;
#3017 = DIRECTION ( 'NONE',  ( 0.000000000000000000, -0.9123518090004800740, -0.4094071037653735923 ) ) ;
#3018 = ORIENTED_EDGE ( 'NONE', *, *, #14425, .F. ) ;
#3019 = CARTESIAN_POINT ( 'NONE',  ( 209.4102522745655506, 3.389308509292514149, -14.00000000000005507 ) ) ;
#3020 = CARTESIAN_POINT ( 'NONE',  ( 221.3323636658532507, 33.48785815289731005, -17.20332536629375753 ) ) ;
#3021 = DIRECTION ( 'NONE',  ( -0.4330127018922105830, -0.2499999999999990563, 0.8660254037844432595 ) ) ;
#3022 = ADVANCED_FACE ( 'NONE', ( #1549 ), #20922, .T. ) ;
#3023 = CARTESIAN_POINT ( 'NONE',  ( 229.1926608780348715, 37.74206926103876469, -16.57782486433073643 ) ) ;
#3024 = B_SPLINE_CURVE_WITH_KNOTS ( 'NONE', 3,
 ( #17955, #6586, #12876, #19331 ),
 .UNSPECIFIED., .F., .F.,
 ( 4, 4 ),
 ( 3.993865398866640540E-07, 0.0006730501785945447674 ),
 .UNSPECIFIED. ) ;
#3025 = EDGE_CURVE ( 'NONE', #15887, #3315, #1761, .T. ) ;
#3026 = EDGE_LOOP ( 'NONE', ( #16299, #19995, #7059, #14450, #19047, #8478 ) ) ;
#3027 = LINE ( 'NONE', #4406, #10175 ) ;
#3028 = ORIENTED_EDGE ( 'NONE', *, *, #9163, .F. ) ;
#3029 = CARTESIAN_POINT ( 'NONE',  ( 98.91428619100412334, 200.0914894846854679, 8.500000000000049738 ) ) ;
#3030 = LINE ( 'NONE', #9474, #15975 ) ;
#3031 = DIRECTION ( 'NONE',  ( -0.5000000000000054401, 0.8660254037844354880, -0.000000000000000000 ) ) ;
#3032 = EDGE_CURVE ( 'NONE', #18332, #12370, #2087, .T. ) ;
#3033 = DIRECTION ( 'NONE',  ( 0.8660254037844370423, 0.5000000000000026645, -0.000000000000000000 ) ) ;
#3034 = LINE ( 'NONE', #15679, #13135 ) ;
#3035 = EDGE_LOOP ( 'NONE', ( #1444, #5579, #19457, #13905 ) ) ;
#3036 = CARTESIAN_POINT ( 'NONE',  ( -7.400583024429460366, 65.00000000000000000, -22.49999999999999645 ) ) ;
#3037 = EDGE_CURVE ( 'NONE', #20359, #2239, #2418, .T. ) ;
#3038 = AXIS2_PLACEMENT_3D ( 'NONE', #9596, #11629, #9905 ) ;
#3039 = DIRECTION ( 'NONE',  ( 0.5000000000000044409, -0.8660254037844360431, 0.000000000000000000 ) ) ;
#3040 = CARTESIAN_POINT ( 'NONE',  ( -4.715799786731095899, 45.61903957271908183, -5.387724600985420942 ) ) ;
#3041 = CARTESIAN_POINT ( 'NONE',  ( 209.9458835816058411, 16.63000860489531263, -23.47937149798938350 ) ) ;
#3042 = AXIS2_PLACEMENT_3D ( 'NONE', #14262, #19018, #14469 ) ;
#3043 = EDGE_CURVE ( 'NONE', #8683, #15788, #18074, .T. ) ;
#3044 = DIRECTION ( 'NONE',  ( 0.3430151393149146744, 0.1980398830195856108, 0.9182161068802695558 ) ) ;
#3045 = DIRECTION ( 'NONE',  ( -1.000000000000000000, 0.000000000000000000, 0.000000000000000000 ) ) ;
#3046 = ORIENTED_EDGE ( 'NONE', *, *, #18809, .F. ) ;
#3047 = DIRECTION ( 'NONE',  ( 0.5000000000000046629, -0.8660254037844360431, -4.006172263299081054E-16 ) ) ;
#3048 = CARTESIAN_POINT ( 'NONE',  ( 218.0089219944356671, 37.69763723594765992, -14.00000000000005507 ) ) ;
#3049 = CARTESIAN_POINT ( 'NONE',  ( -15.99999999999999289, 10.09941697557069418, 12.50000000000000000 ) ) ;
#3050 = VERTEX_POINT ( 'NONE', #5429 ) ;
#3051 = VERTEX_POINT ( 'NONE', #8409 ) ;
#3052 = ORIENTED_EDGE ( 'NONE', *, *, #4691, .T. ) ;
#3053 = LINE ( 'NONE', #9507, #2094 ) ;
#3054 = CARTESIAN_POINT ( 'NONE',  ( 219.2795586678252562, 11.24462313530347757, -14.01558723443205068 ) ) ;
#3055 = CARTESIAN_POINT ( 'NONE',  ( 220.2180084519553134, 35.41797800104779270, -14.00000000000005507 ) ) ;
#3056 = VECTOR ( 'NONE', #2798, 1000.000000000000114 ) ;
#3057 = CARTESIAN_POINT ( 'NONE',  ( -28.22616385396477057, 8.915032500921942216, 2.688307159736136764 ) ) ;
#3058 = ORIENTED_EDGE ( 'NONE', *, *, #4826, .F. ) ;
#3059 = EDGE_CURVE ( 'NONE', #13220, #13875, #391, .T. ) ;
#3060 = AXIS2_PLACEMENT_3D ( 'NONE', #2923, #10751, #12262 ) ;
#3061 = ADVANCED_FACE ( 'NONE', ( #6706 ), #5324, .F. ) ;
#3062 = EDGE_LOOP ( 'NONE', ( #6086, #6870, #13066, #11835, #18952 ) ) ;
#3063 = B_SPLINE_CURVE_WITH_KNOTS ( 'NONE', 3,
 ( #20729, #1237, #20310, #7684 ),
 .UNSPECIFIED., .F., .F.,
 ( 4, 4 ),
 ( 2.844611917532930550E-07, 0.0004523377029716283662 ),
 .UNSPECIFIED. ) ;
#3064 = CARTESIAN_POINT ( 'NONE',  ( 26.00000000000000355, 4.171999999999999709, 0.000000000000000000 ) ) ;
#3065 = LINE ( 'NONE', #14424, #12813 ) ;
#3066 = DIRECTION ( 'NONE',  ( 0.000000000000000000, 0.4999999999999985012, -0.8660254037844394848 ) ) ;
#3067 = ADVANCED_FACE ( 'NONE', ( #259 ), #18390, .T. ) ;
#3068 = AXIS2_PLACEMENT_3D ( 'NONE', #4984, #2140, #14673 ) ;
#3069 = CARTESIAN_POINT ( 'NONE',  ( 219.8080624143775594, 36.12802536649407870, -17.81526153211078878 ) ) ;
#3070 = CARTESIAN_POINT ( 'NONE',  ( -31.81656357967666082, 64.12857799857799534, 2.491815815244385224 ) ) ;
#3071 = CARTESIAN_POINT ( 'NONE',  ( 79.27926581092380331, 66.53148362518940928, -25.41189871557945068 ) ) ;
#3072 = AXIS2_PLACEMENT_3D ( 'NONE', #9706, #14832, #16198 ) ;
#3073 = VERTEX_POINT ( 'NONE', #19647 ) ;
#3074 = DIRECTION ( 'NONE',  ( -0.6946590618905486014, -0.4010615963775267523, -0.5971585917027842916 ) ) ;
#3075 = VECTOR ( 'NONE', #13990, 1000.000000000000000 ) ;
#3076 = DIRECTION ( 'NONE',  ( 0.5000000000000054401, -0.8660254037844354880, 0.000000000000000000 ) ) ;
#3077 = DIRECTION ( 'NONE',  ( 0.8660254037844372643, 0.5000000000000027756, -0.000000000000000000 ) ) ;
#3078 = VERTEX_POINT ( 'NONE', #3541 ) ;
#3079 = EDGE_CURVE ( 'NONE', #1467, #19358, #3746, .T. ) ;
#3080 = CARTESIAN_POINT ( 'NONE',  ( 81.73881534337073163, 63.13855879245894442, 0.3687221123209319384 ) ) ;
#3081 = VECTOR ( 'NONE', #4970, 999.9999999999998863 ) ;
#3082 = ORIENTED_EDGE ( 'NONE', *, *, #3899, .T. ) ;
#3083 = ORIENTED_EDGE ( 'NONE', *, *, #5316, .T. ) ;
#3084 = CARTESIAN_POINT ( 'NONE',  ( -3.117832412439754286, 75.18040026313899205, -1.430629151367028395 ) ) ;
#3085 = CARTESIAN_POINT ( 'NONE',  ( 208.0983737146324870, 5.661548828456886895, -14.00000000000005507 ) ) ;
#3086 = CONICAL_SURFACE ( 'NONE', #13240, 10.85470691220533190, 0.8171114040043576665 ) ;
#3087 = EDGE_CURVE ( 'NONE', #11275, #12336, #16583, .T. ) ;
#3088 = VECTOR ( 'NONE', #4887, 1000.000000000000227 ) ;
#3089 = EDGE_CURVE ( 'NONE', #5258, #2325, #16478, .T. ) ;
#3090 = DIRECTION ( 'NONE',  ( 0.5000000000000052180, -0.8660254037844355990, 0.000000000000000000 ) ) ;
#3091 = VECTOR ( 'NONE', #4986, 1000.000000000000000 ) ;
#3092 = CONICAL_SURFACE ( 'NONE', #13931, 4.509097725792825528, 0.5235987755983015912 ) ;
#3093 = CARTESIAN_POINT ( 'NONE',  ( 82.75906001725628869, 150.6134727143929695, 41.00000000000001421 ) ) ;
#3094 = ORIENTED_EDGE ( 'NONE', *, *, #3189, .F. ) ;
#3095 = CARTESIAN_POINT ( 'NONE',  ( 30.10683012259193703, -24.14213562373095456, 0.000000000000000000 ) ) ;
#3096 = DIRECTION ( 'NONE',  ( -0.5566703992264186995, -0.3213938048432738448, -0.7660444431189767922 ) ) ;
#3097 = CARTESIAN_POINT ( 'NONE',  ( 208.9194833127196489, 31.78152281641241572, -14.16331216883973987 ) ) ;
#3098 = LINE ( 'NONE', #6251, #20672 ) ;
#3099 = CARTESIAN_POINT ( 'NONE',  ( 199.2144802262915846, 21.04890371929339921, -14.00000000000005507 ) ) ;
#3100 = FACE_OUTER_BOUND ( 'NONE', #18819, .T. ) ;
#3101 = DIRECTION ( 'NONE',  ( -0.000000000000000000, 1.000000000000000000, -0.000000000000000000 ) ) ;
#3102 = VECTOR ( 'NONE', #7583, 999.9999999999998863 ) ;
#3103 = DIRECTION ( 'NONE',  ( 0.000000000000000000, 6.938893903907178303E-18, 1.000000000000000000 ) ) ;
#3104 = CARTESIAN_POINT ( 'NONE',  ( 190.7433706042750146, 35.72129598111152404, -9.000000000000062172 ) ) ;
#3105 = FACE_OUTER_BOUND ( 'NONE', #16829, .T. ) ;
#3106 = ORIENTED_EDGE ( 'NONE', *, *, #19854, .T. ) ;
#3107 = AXIS2_PLACEMENT_3D ( 'NONE', #10271, #16760, #11998 ) ;
#3108 = AXIS2_PLACEMENT_3D ( 'NONE', #5903, #6113, #18861 ) ;
#3109 = LINE ( 'NONE', #20479, #8122 ) ;
#3110 = CARTESIAN_POINT ( 'NONE',  ( 82.31088920383102447, 65.12868601141531144, 0.6320188806532470727 ) ) ;
#3111 = VECTOR ( 'NONE', #18771, 1000.000000000000114 ) ;
#3112 = CARTESIAN_POINT ( 'NONE',  ( 220.6758428020499139, 34.21305547669431490, -10.54376118423952491 ) ) ;
#3113 = FACE_OUTER_BOUND ( 'NONE', #19423, .T. ) ;
#3115 = EDGE_LOOP ( 'NONE', ( #7105, #12026, #18667, #11764 ) ) ;
#3114 = ORIENTED_EDGE ( 'NONE', *, *, #7465, .T. ) ;
#3116 = CARTESIAN_POINT ( 'NONE',  ( -32.80236296842959121, 72.40585966223045489, 0.5537423545354294152 ) ) ;
#3117 = VERTEX_POINT ( 'NONE', #18277 ) ;
#3118 = CARTESIAN_POINT ( 'NONE',  ( 217.6662657152042186, 37.70637131117752716, -15.46846178913017411 ) ) ;
#3119 = CARTESIAN_POINT ( 'NONE',  ( -29.42634578414424240, 77.12664207850305331, -3.593879484355423592 ) ) ;
#3120 = VECTOR ( 'NONE', #7350, 1000.000000000000000 ) ;
#3121 = DIRECTION ( 'NONE',  ( -0.8660254037844360431, -0.5000000000000044409, 5.976026924694052093E-17 ) ) ;
#3122 = EDGE_CURVE ( 'NONE', #13435, #1201, #10305, .T. ) ;
#3123 = CARTESIAN_POINT ( 'NONE',  ( 61.99529059433388767, 216.5773763115390693, -28.99999999999998934 ) ) ;
#3124 = ORIENTED_EDGE ( 'NONE', *, *, #968, .T. ) ;
#3125 = FACE_OUTER_BOUND ( 'NONE', #17314, .T. ) ;
#3126 = DIRECTION ( 'NONE',  ( 0.000000000000000000, 0.000000000000000000, 1.000000000000000000 ) ) ;
#3127 = VERTEX_POINT ( 'NONE', #1857 ) ;
#3128 = CARTESIAN_POINT ( 'NONE',  ( 65.65554463217814885, 230.2376303493835223, -14.00000000000003020 ) ) ;
#3129 = CARTESIAN_POINT ( 'NONE',  ( 97.00490953756779788, 125.9389375482329569, 55.99999999999997868 ) ) ;
#3130 = ORIENTED_EDGE ( 'NONE', *, *, #3319, .T. ) ;
#3131 = CIRCLE ( 'NONE', #17699, 12.50000000000000000 ) ;
#3132 = DIRECTION ( 'NONE',  ( 0.8660254037844371533, 0.5000000000000026645, -6.661338147750938256E-16 ) ) ;
#3133 = AXIS2_PLACEMENT_3D ( 'NONE', #12116, #2475, #12338 ) ;
#3134 = EDGE_CURVE ( 'NONE', #9243, #18502, #19007, .T. ) ;
#3135 = CIRCLE ( 'NONE', #15008, 6.960520131757800932 ) ;
#3136 = ORIENTED_EDGE ( 'NONE', *, *, #7836, .F. ) ;
#3137 = CARTESIAN_POINT ( 'NONE',  ( 209.4677058171011197, 30.49417139021348078, -11.75443427544081310 ) ) ;
#3138 = DIRECTION ( 'NONE',  ( -0.5000000000000051070, 0.8660254037844359321, -0.000000000000000000 ) ) ;
#3139 = DIRECTION ( 'NONE',  ( -0.5000000000000051070, 0.8660254037844359321, -0.000000000000000000 ) ) ;
#3140 = FACE_OUTER_BOUND ( 'NONE', #1776, .T. ) ;
#3141 = CARTESIAN_POINT ( 'NONE',  ( -27.23257958228011688, 9.698350540763776451, -5.494722669932186498 ) ) ;
#3142 = EDGE_CURVE ( 'NONE', #5200, #12877, #18673, .T. ) ;
#3143 = VERTEX_POINT ( 'NONE', #8302 ) ;
#3144 = EDGE_CURVE ( 'NONE', #19267, #5668, #14174, .T. ) ;
#3145 = CARTESIAN_POINT ( 'NONE',  ( 197.6384891630574430, 5.400333206920676865, -21.69368824361338355 ) ) ;
#3146 = VECTOR ( 'NONE', #10242, 1000.000000000000000 ) ;
#3147 = ORIENTED_EDGE ( 'NONE', *, *, #16761, .T. ) ;
#3148 = CARTESIAN_POINT ( 'NONE',  ( -3.660952356081173420, 47.48533333485243446, -2.023060265137478275 ) ) ;
#3149 = CARTESIAN_POINT ( 'NONE',  ( 4.000000000000000000, -1.759474945355379072, 3.047500000000001652 ) ) ;
#3150 = DIRECTION ( 'NONE',  ( -0.6946590618905487124, -0.4010615963775269188, -0.5971585917027841806 ) ) ;
#3151 = CARTESIAN_POINT ( 'NONE',  ( 97.07523654288182513, 198.7838771924956518, 12.10917801131580163 ) ) ;
#3152 = ORIENTED_EDGE ( 'NONE', *, *, #5974, .F. ) ;
#3153 = ORIENTED_EDGE ( 'NONE', *, *, #14366, .T. ) ;
#3154 = CARTESIAN_POINT ( 'NONE',  ( 195.4355411401220124, 3.951450668684652445, -16.79818413631467067 ) ) ;
#3155 = CARTESIAN_POINT ( 'NONE',  ( 101.0793497004652863, 201.3414894846855248, 11.00000000000001066 ) ) ;
#3156 = CARTESIAN_POINT ( 'NONE',  ( -8.458929403065925001, 80.00000000014364332, -10.01181548797455889 ) ) ;
#3157 = ORIENTED_EDGE ( 'NONE', *, *, #9205, .T. ) ;
#3158 = ORIENTED_EDGE ( 'NONE', *, *, #14937, .F. ) ;
#3159 = CARTESIAN_POINT ( 'NONE',  ( -19.01411426359141288, 59.74405275486697064, -3.991311237440302584 ) ) ;
#3160 = DIRECTION ( 'NONE',  ( -0.8660254037844370423, -0.5000000000000026645, 0.000000000000000000 ) ) ;
#3161 = CARTESIAN_POINT ( 'NONE',  ( -31.82323003959540486, 64.25000000000000000, 2.481238266578627449 ) ) ;
#3162 = CARTESIAN_POINT ( 'NONE',  ( -11.81109483436797269, 62.83286948270322370, -2.731108915583023045 ) ) ;
#3163 = CONICAL_SURFACE ( 'NONE', #9918, 10.85470691220533190, 0.8171114040043576665 ) ;
#3164 = ORIENTED_EDGE ( 'NONE', *, *, #16286, .T. ) ;
#3165 = EDGE_CURVE ( 'NONE', #16570, #5150, #15023, .T. ) ;
#3166 = VERTEX_POINT ( 'NONE', #11610 ) ;
#3167 = CARTESIAN_POINT ( 'NONE',  ( 5.000000000000000000, 3.513898075855363068, 2.028749999999995168 ) ) ;
#3168 = ADVANCED_FACE ( 'NONE', ( #3640 ), #12247, .T. ) ;
#3169 =( NAMED_UNIT ( * ) SI_UNIT ( $, .STERADIAN. ) SOLID_ANGLE_UNIT ( ) );
#3170 = DIRECTION ( 'NONE',  ( -0.4711304610594142517, 0.8160218955482504422, 0.3348796121709773366 ) ) ;
#3171 = LINE ( 'NONE', #14536, #15654 ) ;
#3172 = CARTESIAN_POINT ( 'NONE',  ( 221.2813132983563094, 33.16434981460763964, -11.28015071478347764 ) ) ;
#3173 = DIRECTION ( 'NONE',  ( 0.8660254037844360431, 0.5000000000000045519, 0.000000000000000000 ) ) ;
#3174 = CIRCLE ( 'NONE', #10608, 5.000000000000002665 ) ;
#3175 = AXIS2_PLACEMENT_3D ( 'NONE', #5396, #19718, #10162 ) ;
#3176 = CARTESIAN_POINT ( 'NONE',  ( -27.30495104032085862, 66.33121464498888997, 5.333703082177909671 ) ) ;
#3177 = DIRECTION ( 'NONE',  ( 0.8660254037844372643, 0.5000000000000027756, -0.000000000000000000 ) ) ;
#3178 = DIRECTION ( 'NONE',  ( -0.4758887346169385357, -0.2747544890354034486, 0.8354878114129393740 ) ) ;
#3179 = EDGE_CURVE ( 'NONE', #14733, #18877, #17665, .T. ) ;
#3180 = ORIENTED_EDGE ( 'NONE', *, *, #9539, .T. ) ;
#3181 = CARTESIAN_POINT ( 'NONE',  ( 63.25496377350514621, 81.89610108269177147, -5.027972649527582938 ) ) ;
#3182 = ORIENTED_EDGE ( 'NONE', *, *, #19141, .F. ) ;
#3183 = VERTEX_POINT ( 'NONE', #7032 ) ;
#3184 = CARTESIAN_POINT ( 'NONE',  ( -4.120658645831395184, 73.83089348061646717, 3.891407385553233844 ) ) ;
#3185 = CARTESIAN_POINT ( 'NONE',  ( 217.5096804110553137, 10.22278344732445809, -20.84195174293596153 ) ) ;
#3186 = EDGE_CURVE ( 'NONE', #17982, #10285, #13517, .T. ) ;
#3187 = APPLICATION_PROTOCOL_DEFINITION ( 'draft international standard', 'automotive_design', 1998, #19729 ) ;
#3188 = VECTOR ( 'NONE', #2964, 1000.000000000000227 ) ;
#3189 = EDGE_CURVE ( 'NONE', #11812, #4703, #8506, .T. ) ;
#3190 = CARTESIAN_POINT ( 'NONE',  ( 219.6109973649995197, 35.85150367506854963, -10.49174204642374519 ) ) ;
#3191 = ORIENTED_EDGE ( 'NONE', *, *, #16876, .F. ) ;
#3192 = CARTESIAN_POINT ( 'NONE',  ( 212.6431940553267452, 14.06330361558336861, -5.407152407594061572 ) ) ;
#3193 = CARTESIAN_POINT ( 'NONE',  ( 210.4099586451761184, 28.82287685411301936, -16.37159109994057360 ) ) ;
#3194 = DIRECTION ( 'NONE',  ( -0.8660254037844360431, -0.5000000000000045519, -7.398944170774820286E-15 ) ) ;
#3195 = VERTEX_POINT ( 'NONE', #20593 ) ;
#3196 = DIRECTION ( 'NONE',  ( -0.8660254037844361541, -0.5000000000000045519, 5.976026924694053325E-17 ) ) ;
#3197 = DIRECTION ( 'NONE',  ( 0.5000000000000054401, -0.8660254037844354880, 0.000000000000000000 ) ) ;
#3198 = EDGE_CURVE ( 'NONE', #3359, #9504, #10629, .T. ) ;
#3199 = LINE ( 'NONE', #17023, #2054 ) ;
#3200 = FACE_OUTER_BOUND ( 'NONE', #3619, .T. ) ;
#3201 = EDGE_CURVE ( 'NONE', #7333, #7908, #12457, .T. ) ;
#3202 = VERTEX_POINT ( 'NONE', #14050 ) ;
#3203 = AXIS2_PLACEMENT_3D ( 'NONE', #1735, #3322, #8075 ) ;
#3204 = DIRECTION ( 'NONE',  ( 0.8660254037844352659, 0.5000000000000056621, 0.000000000000000000 ) ) ;
#3205 = CARTESIAN_POINT ( 'NONE',  ( 184.9952905943349606, 3.535126980567709687, -22.00000000000003908 ) ) ;
#3206 = CARTESIAN_POINT ( 'NONE',  ( 220.5718355850134174, 34.18728306015038498, -10.64970491435236788 ) ) ;
#3207 = LINE ( 'NONE', #9343, #20597 ) ;
#3208 = EDGE_CURVE ( 'NONE', #13235, #13711, #13595, .T. ) ;
#3210 = ORIENTED_EDGE ( 'NONE', *, *, #20857, .T. ) ;
#3209 = EDGE_LOOP ( 'NONE', ( #8623, #12957, #8153, #18833 ) ) ;
#3211 = UNCERTAINTY_MEASURE_WITH_UNIT (LENGTH_MEASURE( 1.000000000000000082E-05 ), #2630, 'distance_accuracy_value', 'NONE');
#3212 = ORIENTED_EDGE ( 'NONE', *, *, #3394, .T. ) ;
#3213 = CARTESIAN_POINT ( 'NONE',  ( 22.00490953756710510, 255.8427481158984733, -28.99999999999997513 ) ) ;
#3214 = VERTEX_POINT ( 'NONE', #4066 ) ;
#3215 = EDGE_CURVE ( 'NONE', #20478, #12601, #15337, .T. ) ;
#3216 = CARTESIAN_POINT ( 'NONE',  ( -25.79456020734900790, 80.00000000016163426, -7.778117258978351600 ) ) ;
#3217 = CARTESIAN_POINT ( 'NONE',  ( 195.3111273346253824, 3.525580966981323616, -11.13829696442576811 ) ) ;
#3218 = ORIENTED_EDGE ( 'NONE', *, *, #843, .F. ) ;
#3219 = VECTOR ( 'NONE', #13608, 1000.000000000000114 ) ;
#3220 = CARTESIAN_POINT ( 'NONE',  ( 206.6380630506355089, 25.33491126127989546, -23.06309126349817618 ) ) ;
#3221 = FACE_OUTER_BOUND ( 'NONE', #4011, .T. ) ;
#3222 = CARTESIAN_POINT ( 'NONE',  ( 214.2406644785986600, 14.98560359448187818, -21.57386172707946059 ) ) ;
#3223 = VERTEX_POINT ( 'NONE', #2491 ) ;
#3224 = CARTESIAN_POINT ( 'NONE',  ( 199.3859296228393134, 5.878169164976177363, -24.01557619556968248 ) ) ;
#3225 = CARTESIAN_POINT ( 'NONE',  ( 198.7027818574981666, 10.13880079795527323, -24.25943249057081630 ) ) ;
#3226 = VERTEX_POINT ( 'NONE', #18596 ) ;
#3227 = AXIS2_PLACEMENT_3D ( 'NONE', #10123, #16928, #12061 ) ;
#3228 = CARTESIAN_POINT ( 'NONE',  ( -31.74999999999995737, 5.551115123125782702E-17, 8.000000000000058620 ) ) ;
#3229 = ORIENTED_EDGE ( 'NONE', *, *, #4724, .F. ) ;
#3230 = CIRCLE ( 'NONE', #5242, 12.99999999999999822 ) ;
#3231 = CARTESIAN_POINT ( 'NONE',  ( 200.4318181982995952, 0.1052612498401872959, -21.90921222372413979 ) ) ;
#3232 = DIRECTION ( 'NONE',  ( 0.8660254037844360431, 0.5000000000000044409, -5.976026924694053325E-17 ) ) ;
#3233 = VECTOR ( 'NONE', #7042, 999.9999999999998863 ) ;
#3234 = DIRECTION ( 'NONE',  ( -0.8660254037844362651, -0.5000000000000045519, 5.976026924694053325E-17 ) ) ;
#3235 = CARTESIAN_POINT ( 'NONE',  ( 209.3053130134501885, 4.970768854950152971, -26.10149651730436915 ) ) ;
#3236 = CARTESIAN_POINT ( 'NONE',  ( -30.00000000000023093, 4.999999999999890754, -7.265667520938737134 ) ) ;
#3237 = APPLICATION_CONTEXT ( 'automotive_design' ) ;
#3238 = EDGE_LOOP ( 'NONE', ( #6683, #6477, #9346, #19511, #15256 ) ) ;
#3239 = CARTESIAN_POINT ( 'NONE',  ( 226.6211368133091923, 39.11482588413117867, -14.00000000000005507 ) ) ;
#3240 = ORIENTED_EDGE ( 'NONE', *, *, #11477, .F. ) ;
#3241 = DIRECTION ( 'NONE',  ( -0.5000000000000049960, 0.8660254037844358210, -0.000000000000000000 ) ) ;
#3242 = CARTESIAN_POINT ( 'NONE',  ( -7.804814160866035522, 45.01037650073381968, -9.445069905521446429 ) ) ;
#3243 = CARTESIAN_POINT ( 'NONE',  ( 211.5616548979095626, 6.788689316162965781, -2.044871543907030631 ) ) ;
#3244 = VECTOR ( 'NONE', #10888, 1000.000000000000227 ) ;
#3245 = FACE_BOUND ( 'NONE', #11126, .T. ) ;
#3246 = CARTESIAN_POINT ( 'NONE',  ( 97.54126021093399856, 199.1658384139430495, 12.88365451894100389 ) ) ;
#3248 = ORIENTED_EDGE ( 'NONE', *, *, #6523, .T. ) ;
#3247 = ORIENTED_EDGE ( 'NONE', *, *, #9674, .T. ) ;
#3249 = EDGE_LOOP ( 'NONE', ( #11950, #1982 ) ) ;
#3250 = CARTESIAN_POINT ( 'NONE',  ( 201.7213150758130382, 0.3345463803147161741, -22.69908973750332848 ) ) ;
#3251 = DIRECTION ( 'NONE',  ( -0.8660254037844360431, -0.5000000000000045519, -4.336808689942050277E-16 ) ) ;
#3252 = CARTESIAN_POINT ( 'NONE',  ( -10.93912170749876722, 79.98244021547212412, -11.72107194671489339 ) ) ;
#3253 = VERTEX_POINT ( 'NONE', #2602 ) ;
#3254 = ORIENTED_EDGE ( 'NONE', *, *, #18459, .T. ) ;
#3255 = VERTEX_POINT ( 'NONE', #5644 ) ;
#3256 = EDGE_CURVE ( 'NONE', #139, #7315, #724, .T. ) ;
#3257 = DIRECTION ( 'NONE',  ( -0.5000000000000049960, 0.8660254037844358210, -0.000000000000000000 ) ) ;
#3258 = MANIFOLD_SOLID_BREP ( 'Hex', #16440 ) ;
#3259 = B_SPLINE_CURVE_WITH_KNOTS ( 'NONE', 3,
 ( #5092, #1933, #11574, #13069 ),
 .UNSPECIFIED., .F., .F.,
 ( 4, 4 ),
 ( 3.066983677782642140E-07, 0.0006729574904242660452 ),
 .UNSPECIFIED. ) ;
#3260 = CARTESIAN_POINT ( 'NONE',  ( 220.0061356372121679, 33.65359772315766662, -18.00871210835857994 ) ) ;
#3261 = LINE ( 'NONE', #14635, #2404 ) ;
#3262 = CIRCLE ( 'NONE', #16807, 3.902363844300875240 ) ;
#3263 = DIRECTION ( 'NONE',  ( 1.000000000000000000, 0.000000000000000000, 0.000000000000000000 ) ) ;
#3264 = ORIENTED_EDGE ( 'NONE', *, *, #12504, .T. ) ;
#3265 = ORIENTED_EDGE ( 'NONE', *, *, #18741, .T. ) ;
#3266 = AXIS2_PLACEMENT_3D ( 'NONE', #18734, #3031, #9270 ) ;
#3267 = DIRECTION ( 'NONE',  ( 0.7743856023693681534, 0.000000000000000000, 0.6327139470906508745 ) ) ;
#3268 = AXIS2_PLACEMENT_3D ( 'NONE', #7358, #8954, #10326 ) ;
#3269 = CARTESIAN_POINT ( 'NONE',  ( 229.7450441735844322, 36.78531332789425079, -14.53826389233656968 ) ) ;
#3270 = EDGE_CURVE ( 'NONE', #11034, #20099, #12561, .T. ) ;
#3271 = CARTESIAN_POINT ( 'NONE',  ( 229.4060619913627193, 37.37244769036321657, -10.88971489487124167 ) ) ;
#3272 = CARTESIAN_POINT ( 'NONE',  ( -32.65378408385129916, 58.26992351455638186, 0.9102417315387145713 ) ) ;
#3273 = CARTESIAN_POINT ( 'NONE',  ( -20.99999999999998934, 15.26381062800292199, 11.45643923738960446 ) ) ;
#3274 = DIRECTION ( 'NONE',  ( 0.000000000000000000, -0.000000000000000000, 1.000000000000000000 ) ) ;
#3275 = CARTESIAN_POINT ( 'NONE',  ( -31.74999999999995737, 0.000000000000000000, 6.500000000000000000 ) ) ;
#3276 = CIRCLE ( 'NONE', #2612, 3.902363844300875240 ) ;
#3277 = ORIENTED_EDGE ( 'NONE', *, *, #19740, .F. ) ;
#3278 = ORIENTED_EDGE ( 'NONE', *, *, #9674, .F. ) ;
#3279 = CARTESIAN_POINT ( 'NONE',  ( 60.03527469150965601, 84.37819276222457177, -8.194308862602044385 ) ) ;
#3280 = EDGE_CURVE ( 'NONE', #279, #16948, #6478, .T. ) ;
#3281 = VERTEX_POINT ( 'NONE', #12132 ) ;
#3282 = EDGE_CURVE ( 'NONE', #3474, #20283, #4285, .T. ) ;
#3283 = CARTESIAN_POINT ( 'NONE',  ( 5.000000000000004441, -2.342598717236899830, 4.057500000000059615 ) ) ;
#3284 = CARTESIAN_POINT ( 'NONE',  ( 226.1030387882217667, 42.76698262081583835, -12.55661888456614683 ) ) ;
#3285 = B_SPLINE_CURVE_WITH_KNOTS ( 'NONE', 3,
 ( #7979, #18056, #16066, #11379 ),
 .UNSPECIFIED., .F., .F.,
 ( 4, 4 ),
 ( 2.668860559028547605E-07, 0.0005661931083548105755 ),
 .UNSPECIFIED. ) ;
#3286 = CARTESIAN_POINT ( 'NONE',  ( 52.00490953756739287, 203.8812238888322383, 6.000000000000010658 ) ) ;
#3287 = VERTEX_POINT ( 'NONE', #8940 ) ;
#3288 = CARTESIAN_POINT ( 'NONE',  ( 225.8710342809365557, 42.51582939992156440, -11.94979443502192318 ) ) ;
#3289 = CARTESIAN_POINT ( 'NONE',  ( 219.3291089353582493, 36.33974875727300002, -10.64970491435233058 ) ) ;
#3290 = EDGE_CURVE ( 'NONE', #19358, #20103, #3966, .T. ) ;
#3291 = VERTEX_POINT ( 'NONE', #16899 ) ;
#3292 = CIRCLE ( 'NONE', #8014, 3.902363844300875240 ) ;
#3293 = MANIFOLD_SOLID_BREP ( 'Cut-Extrude9', #11357 ) ;
#3294 = LINE ( 'NONE', #16341, #970 ) ;
#3295 = CARTESIAN_POINT ( 'NONE',  ( 209.8259871216629335, 29.79736469536937093, -16.48372795108025812 ) ) ;
#3296 = CARTESIAN_POINT ( 'NONE',  ( 219.8596994420543922, 35.21110819772844991, -14.00000000000005507 ) ) ;
#3297 = AXIS2_PLACEMENT_3D ( 'NONE', #4960, #16213, #9826 ) ;
#3298 = VERTEX_POINT ( 'NONE', #14270 ) ;
#3299 = CARTESIAN_POINT ( 'NONE',  ( 203.6269058993112253, 1.434739755226664970, -3.662783021451444299 ) ) ;
#3300 = CARTESIAN_POINT ( 'NONE',  ( -15.99999999999999289, 0.000000000000000000, -5.999999999999989342 ) ) ;
#3301 = EDGE_CURVE ( 'NONE', #8955, #13711, #8837, .T. ) ;
#3302 = PLANE ( 'NONE',  #7457 ) ;
#3303 = CARTESIAN_POINT ( 'NONE',  ( 213.4348361543090959, 18.64435631193540388, -18.06789442459603023 ) ) ;
#3304 = CARTESIAN_POINT ( 'NONE',  ( 206.5868379288083645, 3.916477399883220745, -1.717498466822807490 ) ) ;
#3305 = ORIENTED_EDGE ( 'NONE', *, *, #7798, .F. ) ;
#3306 = VERTEX_POINT ( 'NONE', #4800 ) ;
#3307 = DIRECTION ( 'NONE',  ( 0.6634139481689348417, 0.3830222215594926705, -0.6427876096865408062 ) ) ;
#3308 = ADVANCED_FACE ( 'NONE', ( #16250 ), #6272, .F. ) ;
#3309 = CARTESIAN_POINT ( 'NONE',  ( 81.95753769289619584, 65.79275367316732570, 0.6382041694687864419 ) ) ;
#3310 = COLOUR_RGB ( '',0.7921568627450980005, 0.8196078431372548767, 0.9333333333333333481 ) ;
#3311 = DIRECTION ( 'NONE',  ( 0.000000000000000000, 0.8532072764867869585, -0.5215719924900102944 ) ) ;
#3312 = CARTESIAN_POINT ( 'NONE',  ( 78.01023140970075076, 52.17558613751951668, -10.30093800761554412 ) ) ;
#3313 = AXIS2_PLACEMENT_3D ( 'NONE', #17523, #19115, #9234 ) ;
#3315 = VERTEX_POINT ( 'NONE', #19227 ) ;
#3314 = ORIENTED_EDGE ( 'NONE', *, *, #11329, .T. ) ;
#3316 = ORIENTED_EDGE ( 'NONE', *, *, #3433, .F. ) ;
#3317 = EDGE_CURVE ( 'NONE', #9778, #10058, #11277, .T. ) ;
#3318 = CARTESIAN_POINT ( 'NONE',  ( -33.99999999999997868, 64.25000000000000000, -2.528164662410438357 ) ) ;
#3319 = EDGE_CURVE ( 'NONE', #11320, #9010, #4801, .T. ) ;
#3320 = ORIENTED_EDGE ( 'NONE', *, *, #10046, .F. ) ;
#3321 = LINE ( 'NONE', #6276, #11448 ) ;
#3322 = DIRECTION ( 'NONE',  ( -0.000000000000000000, 1.000000000000000000, 1.224646799147353207E-16 ) ) ;
#3323 = VERTEX_POINT ( 'NONE', #6476 ) ;
#3324 = VECTOR ( 'NONE', #1839, 1000.000000000000000 ) ;
#3325 = DIRECTION ( 'NONE',  ( -0.5000000000000054401, 0.8660254037844354880, -0.000000000000000000 ) ) ;
#3326 = B_SPLINE_CURVE_WITH_KNOTS ( 'NONE', 3,
 ( #13757, #2523, #5359, #15469 ),
 .UNSPECIFIED., .F., .F.,
 ( 4, 4 ),
 ( 5.891946918164437828E-05, 0.0007315702612368541607 ),
 .UNSPECIFIED. ) ;
#3327 = EDGE_CURVE ( 'NONE', #11827, #9243, #16062, .T. ) ;
#3328 =( GEOMETRIC_REPRESENTATION_CONTEXT ( 3 ) GLOBAL_UNCERTAINTY_ASSIGNED_CONTEXT ( ( #18710 ) ) GLOBAL_UNIT_ASSIGNED_CONTEXT ( ( #20717, #12570, #12678 ) ) REPRESENTATION_CONTEXT ( 'NONE', 'WORKASPACE' ) );
#3329 = CARTESIAN_POINT ( 'NONE',  ( 61.62883818700242955, 74.84782268386872772, -3.995215303412941399 ) ) ;
#3330 = DIRECTION ( 'NONE',  ( -1.000000000000000000, -0.000000000000000000, -0.000000000000000000 ) ) ;
#3331 = MANIFOLD_SOLID_BREP ( 'Cut-Extrude5', #10659 ) ;
#3332 = EDGE_LOOP ( 'NONE', ( #9932, #7053, #11070, #9704 ) ) ;
#3333 = CARTESIAN_POINT ( 'NONE',  ( 30.00000000000000000, 0.000000000000000000, 28.99999999999999645 ) ) ;
#3334 = VERTEX_POINT ( 'NONE', #141 ) ;
#3335 = DIRECTION ( 'NONE',  ( 0.5566703992264184775, 0.3213938048432735117, 0.7660444431189770143 ) ) ;
#3336 = EDGE_CURVE ( 'NONE', #17269, #3730, #3787, .T. ) ;
#3337 = EDGE_LOOP ( 'NONE', ( #9563, #18671, #15643, #10214 ) ) ;
#3338 = CARTESIAN_POINT ( 'NONE',  ( 209.6745996013020772, 30.08081452043873227, -11.58037181831264029 ) ) ;
#3339 = FACE_OUTER_BOUND ( 'NONE', #11473, .T. ) ;
#3340 = CARTESIAN_POINT ( 'NONE',  ( 216.7438708388689292, 9.007822994031293717, -21.66653917424403986 ) ) ;
#3341 = CARTESIAN_POINT ( 'NONE',  ( -15.99999999999999289, 80.00000000000000000, 0.000000000000000000 ) ) ;
#3342 = DIRECTION ( 'NONE',  ( -0.4758887346169383692, -0.2747544890354036706, 0.8354878114129394850 ) ) ;
#3343 = CARTESIAN_POINT ( 'NONE',  ( 226.1852762309640639, 42.29805313516507681, -11.62239797051690182 ) ) ;
#3344 = VERTEX_POINT ( 'NONE', #1424 ) ;
#3345 = CARTESIAN_POINT ( 'NONE',  ( 79.00508257797014267, 69.14961577860513842, -25.40092402025251062 ) ) ;
#3346 = CARTESIAN_POINT ( 'NONE',  ( -4.095328035041411852, 55.94710214715788510, 3.823182773501264453 ) ) ;
#3347 = AXIS2_PLACEMENT_3D ( 'NONE', #7622, #10592, #1173 ) ;
#3348 = VERTEX_POINT ( 'NONE', #19025 ) ;
#3349 = CARTESIAN_POINT ( 'NONE',  ( -3.469238944213711040, 49.99908011708879485, -12.29405036578229549 ) ) ;
#3350 = CARTESIAN_POINT ( 'NONE',  ( 5.000000000000000000, 4.685197434473812983, -6.938893903907228378E-15 ) ) ;
#3351 = DIRECTION ( 'NONE',  ( 0.5000000000000049960, -0.8660254037844358210, 0.000000000000000000 ) ) ;
#3352 = CARTESIAN_POINT ( 'NONE',  ( 96.97854020012087517, 198.7000365498672920, 11.80616005232970345 ) ) ;
#3354 = ORIENTED_EDGE ( 'NONE', *, *, #13061, .F. ) ;
#3353 = VERTEX_POINT ( 'NONE', #17428 ) ;
#3355 = ORIENTED_EDGE ( 'NONE', *, *, #18858, .F. ) ;
#3356 = CARTESIAN_POINT ( 'NONE',  ( 218.6234151596997322, 10.86579850426016769, -9.718744748713266546 ) ) ;
#3357 = DIRECTION ( 'NONE',  ( -0.8660254037844355990, -0.5000000000000055511, 0.000000000000000000 ) ) ;
#3358 = B_SPLINE_CURVE_WITH_KNOTS ( 'NONE', 3,
 ( #14921, #7255, #8744, #1972, #15242, #19978, #13638, #20091, #16912, #15037, #8536, #12042, #18607, #18289, #13738, #10320, #15139, #11829, #16595, #8639, #5441, #3763, #11940, #18509, #5235, #5552, #13425, #15350 ),
 .UNSPECIFIED., .F., .F.,
 ( 4, 2, 2, 2, 2, 2, 2, 2, 2, 2, 2, 2, 2, 4 ),
 ( 0.004717002832140601738, 0.005306469451344702354, 0.005601202760946753095, 0.005895936070548802969, 0.006485402689752946953, 0.006780135999355018511, 0.007074869308957089202, 0.007369602618559159893, 0.007664335928161231451, 0.008253802547365364159, 0.008548535856967442656, 0.008843269166569519418, 0.009138002476171597915, 0.009432735785773674678 ),
 .UNSPECIFIED. ) ;
#3359 = VERTEX_POINT ( 'NONE', #2906 ) ;
#3360 = CARTESIAN_POINT ( 'NONE',  ( 205.5965122587965084, 9.994899983462953941, -14.00000000000005507 ) ) ;
#3361 = CARTESIAN_POINT ( 'NONE',  ( 214.8451803045405484, 14.80357170752643370, -7.132002368301448847 ) ) ;
#3362 = FACE_OUTER_BOUND ( 'NONE', #13334, .T. ) ;
#3363 = CARTESIAN_POINT ( 'NONE',  ( -15.11132063516011925, 58.47312285553441313, -4.923512665565291435 ) ) ;
#3364 = ORIENTED_EDGE ( 'NONE', *, *, #16554, .F. ) ;
#3365 = ORIENTED_EDGE ( 'NONE', *, *, #13197, .F. ) ;
#3366 = DIRECTION ( 'NONE',  ( 0.8660254037844370423, 0.5000000000000026645, -0.000000000000000000 ) ) ;
#3367 = CARTESIAN_POINT ( 'NONE',  ( 220.5256391327309302, 34.26729766263312627, -17.38313153181864834 ) ) ;
#3368 = AXIS2_PLACEMENT_3D ( 'NONE', #10550, #17528, #1621 ) ;
#3369 = ADVANCED_FACE ( 'NONE', ( #11163 ), #17639, .F. ) ;
#3370 = CARTESIAN_POINT ( 'NONE',  ( 44.99529059433372424, 246.0222400402097946, -18.99999999999997513 ) ) ;
#3371 = CARTESIAN_POINT ( 'NONE',  ( 209.6730417323522033, 12.34848537237979649, -24.85758746085098991 ) ) ;
#3372 = FACE_OUTER_BOUND ( 'NONE', #9626, .T. ) ;
#3373 = ORIENTED_EDGE ( 'NONE', *, *, #5717, .F. ) ;
#3374 = DIRECTION ( 'NONE',  ( -0.8660254037844359321, -0.5000000000000045519, 5.976026924694053325E-17 ) ) ;
#3375 = CARTESIAN_POINT ( 'NONE',  ( 4.000000000000000000, -3.518949890710766581, 4.553649124439118623E-15 ) ) ;
#3376 = ORIENTED_EDGE ( 'NONE', *, *, #13981, .T. ) ;
#3377 = CARTESIAN_POINT ( 'NONE',  ( 61.99846457528121135, 82.86613150643367476, -6.025952610566521095 ) ) ;
#3378 = VECTOR ( 'NONE', #6721, 1000.000000000000000 ) ;
#3379 = VERTEX_POINT ( 'NONE', #3982 ) ;
#3380 = CARTESIAN_POINT ( 'NONE',  ( -15.99999999999998934, 45.63508326896292289, -12.50000000000000000 ) ) ;
#3381 = FACE_OUTER_BOUND ( 'NONE', #5314, .T. ) ;
#3382 = EDGE_CURVE ( 'NONE', #7667, #279, #5467, .T. ) ;
#3383 = VERTEX_POINT ( 'NONE', #18823 ) ;
#3384 = DIRECTION ( 'NONE',  ( 0.8660254037844364872, 0.5000000000000041078, -0.000000000000000000 ) ) ;
#3385 = ITEM_DEFINED_TRANSFORMATION ( 'NONE', 'NONE', #10082,  #18233 ) ;
#3386 = PLANE ( 'NONE',  #471 ) ;
#3387 = ORIENTED_EDGE ( 'NONE', *, *, #12999, .F. ) ;
#3388 = PRESENTATION_LAYER_ASSIGNMENT (  '', '', ( #5407 ) ) ;
#3389 = CYLINDRICAL_SURFACE ( 'NONE', #9093, 12.99999999999999822 ) ;
#3390 = CARTESIAN_POINT ( 'NONE',  ( 182.3972143829816446, 2.035126980567696364, -6.000000000000009770 ) ) ;
#3391 = ADVANCED_FACE ( 'NONE', ( #10431 ), #13611, .T. ) ;
#3392 = CIRCLE ( 'NONE', #13898, 2.499999999999994671 ) ;
#3393 = ORIENTED_EDGE ( 'NONE', *, *, #591, .F. ) ;
#3394 = EDGE_CURVE ( 'NONE', #17439, #15921, #14064, .T. ) ;
#3395 = CARTESIAN_POINT ( 'NONE',  ( 58.57586221349259858, 85.50000000000002842, -12.50000000002017231 ) ) ;
#3396 = CARTESIAN_POINT ( 'NONE',  ( 218.1626406098745008, 38.35320191943676349, -14.00000000000005507 ) ) ;
#3397 = B_SPLINE_CURVE_WITH_KNOTS ( 'NONE', 3,
 ( #2157, #10391, #19945, #5525 ),
 .UNSPECIFIED., .F., .F.,
 ( 4, 4 ),
 ( 3.426792995371261377E-07, 0.0008543284172840702635 ),
 .UNSPECIFIED. ) ;
#3398 = AXIS2_PLACEMENT_3D ( 'NONE', #427, #313, #6759 ) ;
#3399 = DIRECTION ( 'NONE',  ( 0.8660254037844380415, 0.5000000000000008882, 0.000000000000000000 ) ) ;
#3400 = CARTESIAN_POINT ( 'NONE',  ( 206.1084928877312734, 25.02916378517234364, -14.00000000000005329 ) ) ;
#3401 = PLANE ( 'NONE',  #8166 ) ;
#3402 = VERTEX_POINT ( 'NONE', #13740 ) ;
#3403 = CARTESIAN_POINT ( 'NONE',  ( 208.0983737146324870, 5.661548828456886895, -14.00000000000005507 ) ) ;
#3404 = CARTESIAN_POINT ( 'NONE',  ( 60.45545169401432162, 84.05486846333056405, -7.636015506719354917 ) ) ;
#3405 = AXIS2_PLACEMENT_3D ( 'NONE', #14558, #17827, #15934 ) ;
#3406 = ORIENTED_EDGE ( 'NONE', *, *, #10284, .F. ) ;
#3407 = DIRECTION ( 'NONE',  ( 0.4999999999999995004, -0.8660254037844390407, 0.000000000000000000 ) ) ;
#3408 = CIRCLE ( 'NONE', #4757, 11.98469917212512215 ) ;
#3409 = CARTESIAN_POINT ( 'NONE',  ( 75.06184213092844004, 52.04164024659630172, -13.66203483571357147 ) ) ;
#3411 = EDGE_LOOP ( 'NONE', ( #1971, #5989 ) ) ;
#3410 = EDGE_LOOP ( 'NONE', ( #11951, #18593, #4304, #11960 ) ) ;
#3412 = ORIENTED_EDGE ( 'NONE', *, *, #17197, .F. ) ;
#3413 = VECTOR ( 'NONE', #17034, 1000.000000000000114 ) ;
#3414 = ORIENTED_EDGE ( 'NONE', *, *, #8756, .F. ) ;
#3415 = ORIENTED_EDGE ( 'NONE', *, *, #11618, .F. ) ;
#3416 = EDGE_CURVE ( 'NONE', #10783, #3402, #2026, .T. ) ;
#3417 = VECTOR ( 'NONE', #14485, 1000.000000000000227 ) ;
#3418 = DIRECTION ( 'NONE',  ( 0.000000000000000000, -1.000000000000000000, 0.000000000000000000 ) ) ;
#3419 = ORIENTED_EDGE ( 'NONE', *, *, #7177, .F. ) ;
#3420 = DIRECTION ( 'NONE',  ( -0.2961981327260175267, -0.1710100716628331352, 0.9396926207859105373 ) ) ;
#3421 = CARTESIAN_POINT ( 'NONE',  ( 218.9402551536602459, 37.01326326388927157, -16.94731950718122349 ) ) ;
#3422 = EDGE_CURVE ( 'NONE', #1455, #2596, #2718, .T. ) ;
#3423 = VECTOR ( 'NONE', #17452, 1000.000000000000114 ) ;
#3424 = FACE_OUTER_BOUND ( 'NONE', #20462, .T. ) ;
#3425 = AXIS2_PLACEMENT_3D ( 'NONE', #1446, #8731, #2273 ) ;
#3426 = EDGE_CURVE ( 'NONE', #17375, #2098, #9056, .T. ) ;
#3427 = AXIS2_PLACEMENT_3D ( 'NONE', #18271, #12125, #6918 ) ;
#3428 = CARTESIAN_POINT ( 'NONE',  ( 54.97757980634291641, 77.68911581231870400, -9.638134293611450687 ) ) ;
#3429 = DIRECTION ( 'NONE',  ( 0.5000000000000049960, -0.8660254037844358210, 0.000000000000000000 ) ) ;
#3430 = VERTEX_POINT ( 'NONE', #15661 ) ;
#3431 = DIRECTION ( 'NONE',  ( 0.5000000000000007772, -0.8660254037844381525, 0.000000000000000000 ) ) ;
#3432 = CARTESIAN_POINT ( 'NONE',  ( 221.7236785435837021, 32.19223253356614123, -13.56204498775467293 ) ) ;
#3433 = EDGE_CURVE ( 'NONE', #18964, #2773, #2395, .T. ) ;
#3434 = VERTEX_POINT ( 'NONE', #12044 ) ;
#3435 = CARTESIAN_POINT ( 'NONE',  ( 4.000000000000000000, 5.278424836066145431, -3.047500000000006093 ) ) ;
#3436 = AXIS2_PLACEMENT_3D ( 'NONE', #17324, #10525, #9043 ) ;
#3437 = ORIENTED_EDGE ( 'NONE', *, *, #11362, .F. ) ;
#3438 = PLANE ( 'NONE',  #9216 ) ;
#3439 = FACE_OUTER_BOUND ( 'NONE', #2007, .T. ) ;
#3440 = CARTESIAN_POINT ( 'NONE',  ( 32.00490953756718682, 238.5222400402097094, -13.99999999999997335 ) ) ;
#3441 = VECTOR ( 'NONE', #8435, 1000.000000000000114 ) ;
#3442 = EDGE_CURVE ( 'NONE', #4151, #10290, #12261, .T. ) ;
#3443 = AXIS2_PLACEMENT_3D ( 'NONE', #15840, #7658, #20700 ) ;
#3444 = CARTESIAN_POINT ( 'NONE',  ( 202.6090205221545943, 8.270070825110927615, -2.522505859538386908 ) ) ;
#3445 = FACE_OUTER_BOUND ( 'NONE', #20437, .T. ) ;
#3446 = CARTESIAN_POINT ( 'NONE',  ( 220.0952493489292863, 33.49924824681244218, -10.80501622924634830 ) ) ;
#3447 = ORIENTED_EDGE ( 'NONE', *, *, #799, .T. ) ;
#3448 = CARTESIAN_POINT ( 'NONE',  ( 79.50714813094847955, 68.67338619406606881, -25.45940246541340457 ) ) ;
#3449 = ADVANCED_FACE ( 'NONE', ( #2293 ), #10541, .T. ) ;
#3450 = CARTESIAN_POINT ( 'NONE',  ( -4.227323187870518417, 46.07367448256901099, -4.257085792854391038 ) ) ;
#3451 = ADVANCED_FACE ( 'NONE', ( #8747 ), #15931, .T. ) ;
#3452 = VERTEX_POINT ( 'NONE', #20297 ) ;
#3453 = FACE_OUTER_BOUND ( 'NONE', #1782, .T. ) ;
#3454 = CARTESIAN_POINT ( 'NONE',  ( 1.463241080976594333, 52.61850491325280643, -4.024748401076783111 ) ) ;
#3455 = DIRECTION ( 'NONE',  ( -0.7500000000000013323, -0.4330127018922261817, -0.4999999999999918954 ) ) ;
#3456 = CONICAL_SURFACE ( 'NONE', #15339, 3.047499999999999876, 1.047197551196590748 ) ;
#3457 = EDGE_CURVE ( 'NONE', #3281, #17344, #18723, .T. ) ;
#3458 = LINE ( 'NONE', #19558, #17270 ) ;
#3459 = VECTOR ( 'NONE', #2735, 1000.000000000000114 ) ;
#3460 = DIRECTION ( 'NONE',  ( -1.000000000000000000, -0.000000000000000000, -0.000000000000000000 ) ) ;
#3461 = B_SPLINE_CURVE_WITH_KNOTS ( 'NONE', 3,
 ( #1970, #168, #13109, #2185, #3650, #19767, #19553, #19450, #18082, #8208, #18185, #16706, #8417, #10103, #16592, #8534, #15034, #17985, #3450, #493, #16393, #74, #6932, #18286, #13421, #1866, #5134, #8313, #19867, #3761, #10213, #3346, #17884, #1763, #9798, #269, #16287, #6714 ),
 .UNSPECIFIED., .F., .F.,
 ( 4, 2, 2, 2, 2, 2, 2, 2, 2, 2, 2, 2, 2, 2, 2, 2, 2, 2, 4 ),
 ( 0.03718627721641753342, 0.03834690901369668115, 0.03950754081097582887, 0.04182880440553412432, 0.04298943620281327205, 0.04415006800009241977, 0.04647133159465070829, 0.04879259518920900374, 0.05111385878376729919, 0.05343512237832559464, 0.05459575417560474236, 0.05575638597288389009, 0.05807764956744218554, 0.06039891316200048099, 0.06272017675655877644, 0.06504144035111705802, 0.06736270394567535347, 0.06968396754023364892, 0.07432649472935021207 ),
 .UNSPECIFIED. ) ;
#3463 = ORIENTED_EDGE ( 'NONE', *, *, #13556, .F. ) ;
#3462 = ORIENTED_EDGE ( 'NONE', *, *, #19445, .T. ) ;
#3464 = ORIENTED_EDGE ( 'NONE', *, *, #17120, .F. ) ;
#3465 = CARTESIAN_POINT ( 'NONE',  ( 227.8089867185126991, 40.13866320645092856, -10.10863206319041296 ) ) ;
#3466 = CARTESIAN_POINT ( 'NONE',  ( 192.5001239273000806, 6.557694572264193944, -12.41782726985248964 ) ) ;
#3467 = EDGE_CURVE ( 'NONE', #16685, #9014, #14437, .T. ) ;
#3468 = ORIENTED_EDGE ( 'NONE', *, *, #11961, .T. ) ;
#3469 = ORIENTED_EDGE ( 'NONE', *, *, #8484, .F. ) ;
#3470 = CARTESIAN_POINT ( 'NONE',  ( 32.00490953756718682, 238.5222400402097094, -18.99999999999997513 ) ) ;
#3471 = CARTESIAN_POINT ( 'NONE',  ( 28.51452848080068847, 214.5677573683055357, -8.999999999999971578 ) ) ;
#3472 = CARTESIAN_POINT ( 'NONE',  ( 218.4771030458653058, 38.02138444702771380, -12.05101037009747600 ) ) ;
#3473 = DIRECTION ( 'NONE',  ( 0.5000000000000044409, -0.8660254037844360431, -8.673617379884021914E-17 ) ) ;
#3474 = VERTEX_POINT ( 'NONE', #698 ) ;
#3475 = ADVANCED_FACE ( 'NONE', ( #20195 ), #8851, .F. ) ;
#3476 = EDGE_LOOP ( 'NONE', ( #11530, #16484, #10681, #7077 ) ) ;
#3477 = FACE_OUTER_BOUND ( 'NONE', #8979, .T. ) ;
#3478 = AXIS2_PLACEMENT_3D ( 'NONE', #441, #2238, #2344 ) ;
#3479 = AXIS2_PLACEMENT_3D ( 'NONE', #16291, #8211, #11509 ) ;
#3480 = CARTESIAN_POINT ( 'NONE',  ( 190.7433706042750146, 35.72129598111152404, -19.00000000000003908 ) ) ;
#3481 = EDGE_CURVE ( 'NONE', #13669, #11795, #8801, .T. ) ;
#3482 = LINE ( 'NONE', #14850, #4150 ) ;
#3483 = CARTESIAN_POINT ( 'NONE',  ( -28.43714190982515078, 50.99592196919532938, 1.276470960689417788 ) ) ;
#3484 = CARTESIAN_POINT ( 'NONE',  ( 198.8157711536554189, -0.5701500946419610916, -8.415281845791808379 ) ) ;
#3485 = B_SPLINE_CURVE_WITH_KNOTS ( 'NONE', 3,
 ( #11469, #15095, #9860, #550 ),
 .UNSPECIFIED., .F., .F.,
 ( 4, 4 ),
 ( 3.242053695260285290E-07, 0.0008543099433540281762 ),
 .UNSPECIFIED. ) ;
#3486 = ORIENTED_EDGE ( 'NONE', *, *, #17031, .F. ) ;
#3487 = CARTESIAN_POINT ( 'NONE',  ( 204.7687975563032978, 2.094011210776437704, -3.125199447383417262 ) ) ;
#3488 = CARTESIAN_POINT ( 'NONE',  ( -20.31374355284814825, 64.25000000000000000, -2.528164662410438357 ) ) ;
#3489 = ORIENTED_EDGE ( 'NONE', *, *, #14474, .T. ) ;
#3490 = AXIS2_PLACEMENT_3D ( 'NONE', #19583, #2213, #7075 ) ;
#3491 = CARTESIAN_POINT ( 'NONE',  ( 55.43008045110529025, 77.49674724409801740, -8.910180418637997590 ) ) ;
#3492 = ORIENTED_EDGE ( 'NONE', *, *, #14716, .T. ) ;
#3493 = CARTESIAN_POINT ( 'NONE',  ( 207.8614403295549380, 4.652369439064019119, -1.545471579934808215 ) ) ;
#3494 = EDGE_CURVE ( 'NONE', #19831, #15541, #10642, .T. ) ;
#3495 = ORIENTED_EDGE ( 'NONE', *, *, #1142, .T. ) ;
#3496 = DIRECTION ( 'NONE',  ( 0.000000000000000000, 0.000000000000000000, -1.000000000000000000 ) ) ;
#3497 = ORIENTED_EDGE ( 'NONE', *, *, #16531, .T. ) ;
#3498 = DIRECTION ( 'NONE',  ( 0.8660254037844370423, 0.5000000000000026645, -0.000000000000000000 ) ) ;
#3499 = VERTEX_POINT ( 'NONE', #7677 ) ;
#3500 = AXIS2_PLACEMENT_3D ( 'NONE', #12737, #7850, #17616 ) ;
#3501 = DIRECTION ( 'NONE',  ( -0.5000000000000049960, 0.8660254037844358210, -0.000000000000000000 ) ) ;
#3502 = AXIS2_PLACEMENT_3D ( 'NONE', #2944, #9383, #11309 ) ;
#3503 = CARTESIAN_POINT ( 'NONE',  ( 205.8264633344831225, 9.596613037118636669, -14.00000000000005507 ) ) ;
#3504 = DIRECTION ( 'NONE',  ( 0.8660254037844360431, 0.5000000000000045519, 0.000000000000000000 ) ) ;
#3505 = DIRECTION ( 'NONE',  ( -1.000000000000000000, -0.000000000000000000, -0.000000000000000000 ) ) ;
#3506 = B_SPLINE_CURVE_WITH_KNOTS ( 'NONE', 3,
 ( #1812, #4578, #12958, #20681 ),
 .UNSPECIFIED., .F., .F.,
 ( 4, 4 ),
 ( 0.0001303590654009653270, 0.0008030098574441160708 ),
 .UNSPECIFIED. ) ;
#3507 = ORIENTED_EDGE ( 'NONE', *, *, #18487, .F. ) ;
#3508 = DIRECTION ( 'NONE',  ( 0.4439426092011872771, -0.7689311547811458203, 0.4600650377311618078 ) ) ;
#3509 = CARTESIAN_POINT ( 'NONE',  ( 193.1209940990829637, 6.916154133074862820, -9.448537646917497312 ) ) ;
#3510 = CYLINDRICAL_SURFACE ( 'NONE', #15310, 3.902363844300889451 ) ;
#3511 = ORIENTED_EDGE ( 'NONE', *, *, #17990, .T. ) ;
#3512 = LINE ( 'NONE', #14566, #10836 ) ;
#3513 = CARTESIAN_POINT ( 'NONE',  ( 220.6279544895330673, 34.70793063560162750, -17.81526153211079944 ) ) ;
#3514 = CARTESIAN_POINT ( 'NONE',  ( 205.5965122587965084, 9.994899983462953941, -14.00000000000005507 ) ) ;
#3515 = VECTOR ( 'NONE', #4926, 1000.000000000000114 ) ;
#3516 = CARTESIAN_POINT ( 'NONE',  ( 79.56990498979357085, 50.07294208995298135, -8.967104414842829385 ) ) ;
#3518 = VERTEX_POINT ( 'NONE', #20914 ) ;
#3517 = ORIENTED_EDGE ( 'NONE', *, *, #4758, .F. ) ;
#3519 = EDGE_CURVE ( 'NONE', #8913, #14068, #1438, .T. ) ;
#3520 = ORIENTED_EDGE ( 'NONE', *, *, #15423, .T. ) ;
#3521 = DIRECTION ( 'NONE',  ( 0.000000000000000000, 1.000000000000000000, -1.550730178515671504E-16 ) ) ;
#3522 = VERTEX_POINT ( 'NONE', #3224 ) ;
#3523 = PRESENTATION_STYLE_ASSIGNMENT (( #16366 ) ) ;
#3524 = FACE_OUTER_BOUND ( 'NONE', #18859, .T. ) ;
#3525 = CARTESIAN_POINT ( 'NONE',  ( 229.6917281522317751, 36.87765938573448921, -12.97935860811667652 ) ) ;
#3526 = FACE_OUTER_BOUND ( 'NONE', #11437, .T. ) ;
#3527 = VERTEX_POINT ( 'NONE', #12782 ) ;
#3528 = CARTESIAN_POINT ( 'NONE',  ( 218.3216332057867248, 38.08474790828346102, -15.46846178913018477 ) ) ;
#3529 = EDGE_CURVE ( 'NONE', #18580, #15457, #6740, .T. ) ;
#3530 = CARTESIAN_POINT ( 'NONE',  ( 74.49564010550007254, 69.11503523615289168, -0.1607087966260463130 ) ) ;
#3531 = LINE ( 'NONE', #18267, #10055 ) ;
#3532 = EDGE_LOOP ( 'NONE', ( #10982, #17084, #18296 ) ) ;
#3533 = FACE_OUTER_BOUND ( 'NONE', #13747, .T. ) ;
#3534 = DIRECTION ( 'NONE',  ( 0.6000000000000000888, 0.000000000000000000, 0.7999999999999999334 ) ) ;
#3535 = DIRECTION ( 'NONE',  ( 0.5000000000000046629, -0.8660254037844360431, 0.000000000000000000 ) ) ;
#3536 = ADVANCED_FACE ( 'NONE', ( #14175 ), #6190, .F. ) ;
#3538 = ORIENTED_EDGE ( 'NONE', *, *, #17867, .T. ) ;
#3537 = EDGE_LOOP ( 'NONE', ( #2492, #12281, #5509, #3824 ) ) ;
#3539 = ADVANCED_FACE ( 'NONE', ( #4816, #8081 ), #10977, .T. ) ;
#3540 = LINE ( 'NONE', #10093, #15312 ) ;
#3541 = CARTESIAN_POINT ( 'NONE',  ( 5.000000000000000000, 2.342598717236913153, 4.057499999999995666 ) ) ;
#3542 = DIRECTION ( 'NONE',  ( 0.8660254037844375974, 0.5000000000000018874, 0.000000000000000000 ) ) ;
#3543 = CONICAL_SURFACE ( 'NONE', #4569, 13.07248899748297433, 0.6693469023067423196 ) ;
#3544 = CARTESIAN_POINT ( 'NONE',  ( 82.91030674320427352, 62.98464439186960107, -25.48828433254854176 ) ) ;
#3545 = LINE ( 'NONE', #13208, #5999 ) ;
#3546 = DIRECTION ( 'NONE',  ( -0.3200921998322431850, 0.5544159532159285142, 0.7682212795973754060 ) ) ;
#3547 = ORIENTED_EDGE ( 'NONE', *, *, #13844, .T. ) ;
#3548 = ADVANCED_FACE ( 'NONE', ( #12469 ), #6078, .F. ) ;
#3549 = CARTESIAN_POINT ( 'NONE',  ( 75.99050373817134130, 68.37836398556720496, -25.05701615029671459 ) ) ;
#3550 = DIRECTION ( 'NONE',  ( -0.8660254037844380415, -0.5000000000000014433, -0.000000000000000000 ) ) ;
#3551 = EDGE_LOOP ( 'NONE', ( #14830, #16820, #4178, #4256, #12484 ) ) ;
#3552 = FILL_AREA_STYLE_COLOUR ( '', #8187 ) ;
#3553 = CARTESIAN_POINT ( 'NONE',  ( -3.500383879130120501, 49.05626247071266732, -0.2969177088905650685 ) ) ;
#3554 = DIRECTION ( 'NONE',  ( 0.000000000000000000, 0.000000000000000000, 1.000000000000000000 ) ) ;
#3555 = EDGE_CURVE ( 'NONE', #8280, #12773, #19242, .T. ) ;
#3556 = DIRECTION ( 'NONE',  ( 0.5000000000000051070, -0.8660254037844359321, 0.000000000000000000 ) ) ;
#3557 = CARTESIAN_POINT ( 'NONE',  ( 72.49529059433406530, 198.3908428320658288, 11.00000000000001066 ) ) ;
#3558 = LINE ( 'NONE', #19985, #4908 ) ;
#3559 = AXIS2_PLACEMENT_3D ( 'NONE', #18463, #13907, #10606 ) ;
#3561 = EDGE_LOOP ( 'NONE', ( #6545, #20756, #9762, #7156 ) ) ;
#3560 = VERTEX_POINT ( 'NONE', #6388 ) ;
#3562 = ORIENTED_EDGE ( 'NONE', *, *, #1060, .F. ) ;
#3563 = VERTEX_POINT ( 'NONE', #18925 ) ;
#3564 = CARTESIAN_POINT ( 'NONE',  ( 5.000000000000004441, -2.342598717236899830, 4.057500000000059615 ) ) ;
#3565 = CARTESIAN_POINT ( 'NONE',  ( 31.00000000000000711, 65.00000000000000000, -12.50000000000000000 ) ) ;
#3566 = EDGE_CURVE ( 'NONE', #20478, #2569, #12575, .T. ) ;
#3567 = ORIENTED_EDGE ( 'NONE', *, *, #16034, .T. ) ;
#3568 = ORIENTED_EDGE ( 'NONE', *, *, #12310, .T. ) ;
#3569 = CARTESIAN_POINT ( 'NONE',  ( -17.71827568934370234, 58.74352212083275759, -4.698501153746496684 ) ) ;
#3570 = DIRECTION ( 'NONE',  ( -0.000000000000000000, 1.000000000000000000, -0.000000000000000000 ) ) ;
#3571 = CARTESIAN_POINT ( 'NONE',  ( -12.00855099916729607, 61.81641395294881391, -3.013858250467857491 ) ) ;
#3572 = ORIENTED_EDGE ( 'NONE', *, *, #5248, .F. ) ;
#3573 = EDGE_LOOP ( 'NONE', ( #13092, #16124, #6681, #16074 ) ) ;
#3574 = DIRECTION ( 'NONE',  ( 0.2883401610574307661, -0.4994198088140612835, 0.8169698930104472012 ) ) ;
#3575 = EDGE_CURVE ( 'NONE', #11395, #13335, #8443, .T. ) ;
#3576 = VERTEX_POINT ( 'NONE', #20814 ) ;
#3577 = ADVANCED_FACE ( 'NONE', ( #17443 ), #5977, .T. ) ;
#3578 = VECTOR ( 'NONE', #7392, 1000.000000000000000 ) ;
#3579 = AXIS2_PLACEMENT_3D ( 'NONE', #11778, #3920, #16653 ) ;
#3580 = DIRECTION ( 'NONE',  ( -1.000000000000000000, 0.000000000000000000, 0.000000000000000000 ) ) ;
#3581 = LINE ( 'NONE', #17911, #12950 ) ;
#3582 = CARTESIAN_POINT ( 'NONE',  ( -33.28040837221767845, 51.87854031905991548, -5.222875071459978535 ) ) ;
#3583 = CARTESIAN_POINT ( 'NONE',  ( -18.22437098228045116, 19.58037170849552311, 12.30137062747990306 ) ) ;
#3584 = EDGE_CURVE ( 'NONE', #20836, #17213, #4277, .T. ) ;
#3585 = VERTEX_POINT ( 'NONE', #12884 ) ;
#3586 = CARTESIAN_POINT ( 'NONE',  ( 42.30949999999999989, 0.000000000000000000, 0.000000000000000000 ) ) ;
#3587 = DIRECTION ( 'NONE',  ( -0.4999999999999995004, 0.8660254037844390407, 0.000000000000000000 ) ) ;
#3588 = ORIENTED_EDGE ( 'NONE', *, *, #12543, .T. ) ;
#3589 = CARTESIAN_POINT ( 'NONE',  ( 59.88327620991913847, 84.49511162386195906, -8.417773832668045131 ) ) ;
#3590 = VERTEX_POINT ( 'NONE', #15858 ) ;
#3591 = VECTOR ( 'NONE', #6222, 1000.000000000000000 ) ;
#3592 = CARTESIAN_POINT ( 'NONE',  ( 198.5778388975847690, -0.9651341984995248646, -18.20125362229437016 ) ) ;
#3593 = AXIS2_PLACEMENT_3D ( 'NONE', #9731, #17805, #5 ) ;
#3594 = PLANE ( 'NONE',  #2243 ) ;
#3595 = EDGE_CURVE ( 'NONE', #6648, #16240, #11289, .T. ) ;
#3596 = ORIENTED_EDGE ( 'NONE', *, *, #17893, .T. ) ;
#3597 = CARTESIAN_POINT ( 'NONE',  ( 58.37797649651341203, 276.8427481158987007, -26.99999999999999289 ) ) ;
#3598 = CONTEXT_DEPENDENT_SHAPE_REPRESENTATION ( #5800, #6852 ) ;
#3599 = CARTESIAN_POINT ( 'NONE',  ( -4.701390418375630986, 65.75000000000000000, 5.347094680480811490 ) ) ;
#3600 = ORIENTED_EDGE ( 'NONE', *, *, #20802, .F. ) ;
#3601 = DIRECTION ( 'NONE',  ( 0.8660254037844368202, 0.5000000000000031086, 1.665334536937734564E-16 ) ) ;
#3602 = CARTESIAN_POINT ( 'NONE',  ( 197.7577498960094431, 5.469188423194260906, -6.376588578941773555 ) ) ;
#3603 = CIRCLE ( 'NONE', #14475, 11.94520687646042667 ) ;
#3604 = ORIENTED_EDGE ( 'NONE', *, *, #7207, .F. ) ;
#3605 = CARTESIAN_POINT ( 'NONE',  ( 61.99529059433388767, 216.5773763115390693, 1.000000000000017097 ) ) ;
#3606 = DIRECTION ( 'NONE',  ( 0.8660254037844355990, 0.5000000000000054401, 0.000000000000000000 ) ) ;
#3607 = ORIENTED_EDGE ( 'NONE', *, *, #17908, .F. ) ;
#3608 = LINE ( 'NONE', #19819, #6432 ) ;
#3609 = CARTESIAN_POINT ( 'NONE',  ( 32.39721438298033007, 261.8427481158985302, -5.999999999999973355 ) ) ;
#3610 = CARTESIAN_POINT ( 'NONE',  ( 206.7336986317416176, 3.743653614488819503, -1.889534153981315523 ) ) ;
#3611 = ORIENTED_EDGE ( 'NONE', *, *, #7381, .T. ) ;
#3612 = DIRECTION ( 'NONE',  ( 0.5000000000000051070, -0.8660254037844359321, 0.000000000000000000 ) ) ;
#3613 = CARTESIAN_POINT ( 'NONE',  ( 46.88067919638974956, 212.7566511894377754, 48.96815749462641065 ) ) ;
#3614 = CARTESIAN_POINT ( 'NONE',  ( 30.00000000000000355, -10.00000000000000000, -30.00000000000000000 ) ) ;
#3615 = CARTESIAN_POINT ( 'NONE',  ( 75.13664552285537468, 52.14064219013824442, -10.52251561064948682 ) ) ;
#3617 = ORIENTED_EDGE ( 'NONE', *, *, #3481, .T. ) ;
#3616 = EDGE_LOOP ( 'NONE', ( #20907, #12580, #14039, #2437 ) ) ;
#3618 = VECTOR ( 'NONE', #8992, 1000.000000000000227 ) ;
#3619 = EDGE_LOOP ( 'NONE', ( #16905, #16608, #240, #2220 ) ) ;
#3620 = ORIENTED_EDGE ( 'NONE', *, *, #15618, .F. ) ;
#3621 = CARTESIAN_POINT ( 'NONE',  ( 212.9776690748797989, 18.38041077556222191, -19.29168348739316130 ) ) ;
#3622 = ORIENTED_EDGE ( 'NONE', *, *, #14406, .T. ) ;
#3623 = CARTESIAN_POINT ( 'NONE',  ( 204.7012550509497260, 2.055015527128745578, -24.96223045542551233 ) ) ;
#3624 = CARTESIAN_POINT ( 'NONE',  ( -24.58391324610231266, 79.99999999992814992, -9.098350519373951784 ) ) ;
#3625 = CARTESIAN_POINT ( 'NONE',  ( 10.40000000000000568, 3.469446951953588921E-17, 5.000000000000000000 ) ) ;
#3626 = DIRECTION ( 'NONE',  ( -0.000000000000000000, 1.000000000000000000, -0.000000000000000000 ) ) ;
#3627 = ORIENTED_EDGE ( 'NONE', *, *, #12635, .F. ) ;
#3628 = CARTESIAN_POINT ( 'NONE',  ( 219.0871984830704662, 10.36074384021052985, -12.62839849932177394 ) ) ;
#3629 = CARTESIAN_POINT ( 'NONE',  ( 208.0983737146324870, 5.661548828456886895, -14.00000000000005507 ) ) ;
#3630 =( GEOMETRIC_REPRESENTATION_CONTEXT ( 3 ) GLOBAL_UNCERTAINTY_ASSIGNED_CONTEXT ( ( #3211 ) ) GLOBAL_UNIT_ASSIGNED_CONTEXT ( ( #2630, #19149, #10990 ) ) REPRESENTATION_CONTEXT ( 'NONE', 'WORKASPACE' ) );
#3631 = ADVANCED_FACE ( 'NONE', ( #17341 ), #20642, .F. ) ;
#3632 = CARTESIAN_POINT ( 'NONE',  ( 69.99529059433403688, 202.7209698509880411, 11.00000000000001066 ) ) ;
#3633 = ORIENTED_EDGE ( 'NONE', *, *, #10450, .F. ) ;
#3634 = CARTESIAN_POINT ( 'NONE',  ( 1.500000000000001332, 0.000000000000000000, 0.000000000000000000 ) ) ;
#3636 = PLANE ( 'NONE',  #6095 ) ;
#3635 = VECTOR ( 'NONE', #11386, 1000.000000000000227 ) ;
#3637 = DIRECTION ( 'NONE',  ( 0.000000000000000000, 0.000000000000000000, 1.000000000000000000 ) ) ;
#3638 = CARTESIAN_POINT ( 'NONE',  ( -6.118771807841490329, 79.85840876778712527, -10.43301765575355233 ) ) ;
#3639 = ORIENTED_EDGE ( 'NONE', *, *, #11565, .F. ) ;
#3640 = FACE_OUTER_BOUND ( 'NONE', #10474, .T. ) ;
#3641 = FACE_OUTER_BOUND ( 'NONE', #11418, .T. ) ;
#3642 = EDGE_CURVE ( 'NONE', #16030, #2546, #10861, .T. ) ;
#3643 = CARTESIAN_POINT ( 'NONE',  ( 82.75100189971391274, 60.33120646178909396, -24.98450340712203044 ) ) ;
#3644 =( GEOMETRIC_REPRESENTATION_CONTEXT ( 3 ) GLOBAL_UNCERTAINTY_ASSIGNED_CONTEXT ( ( #16361 ) ) GLOBAL_UNIT_ASSIGNED_CONTEXT ( ( #12219, #1089, #15522 ) ) REPRESENTATION_CONTEXT ( 'NONE', 'WORKASPACE' ) );
#3645 =( NAMED_UNIT ( * ) SI_UNIT ( $, .STERADIAN. ) SOLID_ANGLE_UNIT ( ) );
#3646 = CARTESIAN_POINT ( 'NONE',  ( 49.01452848080095492, 179.0607158131434460, 11.00000000000001066 ) ) ;
#3647 = ORIENTED_EDGE ( 'NONE', *, *, #3923, .F. ) ;
#3648 = VECTOR ( 'NONE', #4240, 1000.000000000000227 ) ;
#3649 = CARTESIAN_POINT ( 'NONE',  ( 82.19612864528707519, 65.36250969618502893, -25.63618266340674978 ) ) ;
#3650 = CARTESIAN_POINT ( 'NONE',  ( -14.06953418112486887, 45.58387777135212815, -12.35599831547759742 ) ) ;
#3651 = ADVANCED_FACE ( 'NONE', ( #2823 ), #677, .F. ) ;
#3652 = VERTEX_POINT ( 'NONE', #10086 ) ;
#3653 = EDGE_CURVE ( 'NONE', #7395, #142, #20455, .T. ) ;
#3654 = CARTESIAN_POINT ( 'NONE',  ( 1.431553936783702685, 52.41835994622631745, -4.324939117741945616 ) ) ;
#3655 = CARTESIAN_POINT ( 'NONE',  ( -6.896700228544379030, 79.90031512599163932, -10.76368999076717436 ) ) ;
#3656 = CARTESIAN_POINT ( 'NONE',  ( 195.7290327299236594, 3.943881439888561324, -18.20503500338657688 ) ) ;
#3657 = DIRECTION ( 'NONE',  ( 0.8660254037844370423, 0.5000000000000026645, -0.000000000000000000 ) ) ;
#3658 = CARTESIAN_POINT ( 'NONE',  ( 205.5286554512480848, 3.047921609845726465, -25.78004855466121370 ) ) ;
#3659 = AXIS2_PLACEMENT_3D ( 'NONE', #8047, #17727, #11456 ) ;
#3661 = ORIENTED_EDGE ( 'NONE', *, *, #5748, .F. ) ;
#3660 = ORIENTED_EDGE ( 'NONE', *, *, #5754, .T. ) ;
#3662 = ORIENTED_EDGE ( 'NONE', *, *, #1664, .T. ) ;
#3663 = LINE ( 'NONE', #11635, #7812 ) ;
#3664 = CARTESIAN_POINT ( 'NONE',  ( 79.18111854763493795, 156.8106491262847157, 41.00000000000001421 ) ) ;
#3665 = VERTEX_POINT ( 'NONE', #2059 ) ;
#3666 = ADVANCED_FACE ( 'NONE', ( #19638 ), #16471, .F. ) ;
#3667 = CARTESIAN_POINT ( 'NONE',  ( 79.78236940327508364, 58.62749654732350280, -1.141850372723110629 ) ) ;
#3668 = DIRECTION ( 'NONE',  ( 0.4988343845952719624, -0.8640064986813588144, 0.06824241336467461172 ) ) ;
#3669 = DIRECTION ( 'NONE',  ( 0.000000000000000000, -0.8532072764867869585, 0.5215719924900102944 ) ) ;
#3670 = EDGE_LOOP ( 'NONE', ( #15897, #15746, #17996, #10995, #8406 ) ) ;
#3671 = DIRECTION ( 'NONE',  ( 0.000000000000000000, 0.7775157341893068619, 0.6288634852557930532 ) ) ;
#3672 = DIRECTION ( 'NONE',  ( 0.8660254037844380415, 0.5000000000000014433, 0.000000000000000000 ) ) ;
#3673 = ADVANCED_FACE ( 'NONE', ( #14903 ), #11807, .F. ) ;
#3674 = AXIS2_PLACEMENT_3D ( 'NONE', #1478, #12619, #4958 ) ;
#3675 = CARTESIAN_POINT ( 'NONE',  ( 213.2304086110926278, 13.87128283563446018, -4.915515517929359035 ) ) ;
#3676 = ADVANCED_FACE ( 'NONE', ( #18269 ), #8402, .F. ) ;
#3677 = DIRECTION ( 'NONE',  ( 0.8660254037844362651, 0.5000000000000043299, 0.000000000000000000 ) ) ;
#3678 = CARTESIAN_POINT ( 'NONE',  ( -27.92487288654064059, 52.24757969830196203, -4.564036982978468160 ) ) ;
#3679 = CARTESIAN_POINT ( 'NONE',  ( 207.0179943350028395, 10.81559304280891531, -15.68675928846492695 ) ) ;
#3680 = ORIENTED_EDGE ( 'NONE', *, *, #19974, .T. ) ;
#3681 = CARTESIAN_POINT ( 'NONE',  ( 32.39721438298033007, 261.8427481158985302, -5.999999999999973355 ) ) ;
#3682 = DIRECTION ( 'NONE',  ( -0.000000000000000000, -1.000000000000000000, -0.000000000000000000 ) ) ;
#3684 = ORIENTED_EDGE ( 'NONE', *, *, #1917, .F. ) ;
#3683 = ORIENTED_EDGE ( 'NONE', *, *, #6658, .T. ) ;
#3685 = CARTESIAN_POINT ( 'NONE',  ( 62.90924860651898598, 77.99809401039773604, -12.47726437862388948 ) ) ;
#3686 = EDGE_CURVE ( 'NONE', #10275, #15281, #5117, .T. ) ;
#3687 = ORIENTED_EDGE ( 'NONE', *, *, #17308, .T. ) ;
#3688 = EDGE_CURVE ( 'NONE', #4749, #8514, #18609, .T. ) ;
#3689 = VECTOR ( 'NONE', #4347, 1000.000000000000227 ) ;
#3690 = EDGE_LOOP ( 'NONE', ( #12816, #10856, #15069, #3180 ) ) ;
#3691 = CARTESIAN_POINT ( 'NONE',  ( 203.1960812450809897, 12.73300840892584063, -2.187257959407754804 ) ) ;
#3692 = DIRECTION ( 'NONE',  ( -0.5000000000000051070, 0.8660254037844359321, -0.000000000000000000 ) ) ;
#3693 = ORIENTED_EDGE ( 'NONE', *, *, #5697, .T. ) ;
#3694 = CARTESIAN_POINT ( 'NONE',  ( 7.999999999999998224, 6.500000000000000000, 0.000000000000000000 ) ) ;
#3695 = ORIENTED_EDGE ( 'NONE', *, *, #11551, .T. ) ;
#3696 = CONTEXT_DEPENDENT_SHAPE_REPRESENTATION ( #9726, #20413 ) ;
#3697 = EDGE_CURVE ( 'NONE', #20933, #1032, #7793, .T. ) ;
#3698 = DIRECTION ( 'NONE',  ( -0.5000000000000025535, 0.8660254037844372643, 0.000000000000000000 ) ) ;
#3699 = ORIENTED_EDGE ( 'NONE', *, *, #8610, .F. ) ;
#3700 = MANIFOLD_SOLID_BREP ( 'Chamfer2', #9312 ) ;
#3701 = CARTESIAN_POINT ( 'NONE',  ( 49.86389338619021316, 127.5895726428436205, -12.50000000000000000 ) ) ;
#3702 = CARTESIAN_POINT ( 'NONE',  ( 227.0505393086274637, 40.79937352273880435, -17.59914077799767540 ) ) ;
#3703 = DIRECTION ( 'NONE',  ( 0.8660254037844372643, 0.5000000000000027756, -0.000000000000000000 ) ) ;
#3704 = DIRECTION ( 'NONE',  ( 0.000000000000000000, -6.938893903907177533E-18, -1.000000000000000000 ) ) ;
#3705 = VECTOR ( 'NONE', #20609, 1000.000000000000000 ) ;
#3706 = EDGE_CURVE ( 'NONE', #10070, #19834, #15946, .T. ) ;
#3707 = CARTESIAN_POINT ( 'NONE',  ( 59.50490953756747103, 190.8908428320656867, 11.00000000000001066 ) ) ;
#3708 = VECTOR ( 'NONE', #7049, 1000.000000000000114 ) ;
#3709 = DIRECTION ( 'NONE',  ( -1.000000000000000000, -0.000000000000000000, -0.000000000000000000 ) ) ;
#3710 = DIRECTION ( 'NONE',  ( 0.5000000000000044409, -0.8660254037844360431, -4.006172263299080068E-16 ) ) ;
#3711 = VERTEX_POINT ( 'NONE', #11704 ) ;
#3712 = CARTESIAN_POINT ( 'NONE',  ( -1.794545525815418596, 65.74999999999998579, 2.744335235139482965 ) ) ;
#3713 = ADVANCED_FACE ( 'NONE', ( #9880 ), #16944, .T. ) ;
#3714 = B_SPLINE_CURVE_WITH_KNOTS ( 'NONE', 3,
 ( #2737, #13871, #727, #5578 ),
 .UNSPECIFIED., .F., .F.,
 ( 4, 4 ),
 ( 3.220132087640094245E-07, 0.0008543077511937698446 ),
 .UNSPECIFIED. ) ;
#3715 = CARTESIAN_POINT ( 'NONE',  ( -12.09671107471471707, 68.50841174652784105, -3.129485610713131027 ) ) ;
#3716 = CARTESIAN_POINT ( 'NONE',  ( 75.96605662148094495, 53.24384717281555623, -18.14283704812129017 ) ) ;
#3718 = ORIENTED_EDGE ( 'NONE', *, *, #3584, .F. ) ;
#3717 = VERTEX_POINT ( 'NONE', #18167 ) ;
#3719 = EDGE_CURVE ( 'NONE', #3590, #3344, #16576, .T. ) ;
#3720 = AXIS2_PLACEMENT_3D ( 'NONE', #14151, #14365, #11055 ) ;
#3721 = ORIENTED_EDGE ( 'NONE', *, *, #9073, .F. ) ;
#3722 = VECTOR ( 'NONE', #16890, 1000.000000000000114 ) ;
#3723 = DIRECTION ( 'NONE',  ( 0.5000000000000058842, -0.8660254037844352659, 0.000000000000000000 ) ) ;
#3724 = ORIENTED_EDGE ( 'NONE', *, *, #18207, .F. ) ;
#3725 = CARTESIAN_POINT ( 'NONE',  ( 81.72727647338570023, 63.41126555804013520, -25.40372688915182664 ) ) ;
#3726 = CARTESIAN_POINT ( 'NONE',  ( -16.26048471067390011, 79.99999999999998579, -12.50000000001717204 ) ) ;
#3727 = DIRECTION ( 'NONE',  ( 0.8660254037844352659, 0.5000000000000056621, 0.000000000000000000 ) ) ;
#3728 = CARTESIAN_POINT ( 'NONE',  ( 85.37797649651368204, 230.0773763115391262, -26.99999999999999289 ) ) ;
#3729 = VECTOR ( 'NONE', #12079, 1000.000000000000000 ) ;
#3730 = VERTEX_POINT ( 'NONE', #18068 ) ;
#3731 = CARTESIAN_POINT ( 'NONE',  ( 79.18111854763493795, 156.8106491262847157, 41.00000000000001421 ) ) ;
#3732 = VECTOR ( 'NONE', #19608, 1000.000000000000000 ) ;
#3733 = FACE_OUTER_BOUND ( 'NONE', #5121, .T. ) ;
#3734 = CARTESIAN_POINT ( 'NONE',  ( 159.9952905943348469, 46.83639716978957068, 0.9999999999999386047 ) ) ;
#3735 = ORIENTED_EDGE ( 'NONE', *, *, #4294, .F. ) ;
#3736 = AXIS2_PLACEMENT_3D ( 'NONE', #17475, #4431, #12705 ) ;
#3737 = DIRECTION ( 'NONE',  ( 0.000000000000000000, 0.000000000000000000, 1.000000000000000000 ) ) ;
#3738 = DIRECTION ( 'NONE',  ( 0.5000000000000047740, -0.8660254037844359321, 0.000000000000000000 ) ) ;
#3739 = CIRCLE ( 'NONE', #15621, 3.619616396367202782 ) ;
#3740 = CYLINDRICAL_SURFACE ( 'NONE', #13952, 4.999999999999997335 ) ;
#3741 = CARTESIAN_POINT ( 'NONE',  ( -5.443139766541319702, 79.99999999967708675, -6.747797645777612097 ) ) ;
#3742 = VECTOR ( 'NONE', #95, 1000.000000000000114 ) ;
#3743 = ORIENTED_EDGE ( 'NONE', *, *, #3442, .F. ) ;
#3744 = ORIENTED_EDGE ( 'NONE', *, *, #9979, .T. ) ;
#3745 = DIRECTION ( 'NONE',  ( 0.000000000000000000, 0.000000000000000000, 1.000000000000000000 ) ) ;
#3746 = LINE ( 'NONE', #3858, #20028 ) ;
#3747 = DIRECTION ( 'NONE',  ( 0.4999999999999995004, -0.8660254037844390407, 0.000000000000000000 ) ) ;
#3748 = VECTOR ( 'NONE', #14434, 1000.000000000000000 ) ;
#3749 = AXIS2_PLACEMENT_3D ( 'NONE', #10337, #18523, #7063 ) ;
#3750 = CARTESIAN_POINT ( 'NONE',  ( 79.74209024524658673, 50.54664088538957856, -17.24859437997715972 ) ) ;
#3751 = ADVANCED_FACE ( 'NONE', ( #3533 ), #9976, .F. ) ;
#3752 = CARTESIAN_POINT ( 'NONE',  ( -29.99999999999999645, 5.000000000000000000, 6.407083732717120839 ) ) ;
#3753 = AXIS2_PLACEMENT_3D ( 'NONE', #6462, #231, #11676 ) ;
#3754 = SHAPE_REPRESENTATION_RELATIONSHIP ( 'NONE' , 'NONE' ,  #9638, #5517 ) ;
#3755 = DIRECTION ( 'NONE',  ( 0.000000000000000000, 0.000000000000000000, 1.000000000000000000 ) ) ;
#3756 = VERTEX_POINT ( 'NONE', #15220 ) ;
#3757 = VERTEX_POINT ( 'NONE', #5535 ) ;
#3758 = AXIS2_PLACEMENT_3D ( 'NONE', #9685, #6391, #3535 ) ;
#3759 = ADVANCED_BREP_SHAPE_REPRESENTATION ( '', ( #17281, #18233 ), #2321 ) ;
#3760 = CARTESIAN_POINT ( 'NONE',  ( 81.86472787884530078, 64.82771547793723244, -25.50399698552627115 ) ) ;
#3761 = CARTESIAN_POINT ( 'NONE',  ( -3.843826630376830256, 53.82522964764072526, 2.934722157913033591 ) ) ;
#3762 = ORIENTED_EDGE ( 'NONE', *, *, #16561, .F. ) ;
#3763 = CARTESIAN_POINT ( 'NONE',  ( 201.8742535751798073, 26.32928792145338548, -14.75325243452065749 ) ) ;
#3764 = CARTESIAN_POINT ( 'NONE',  ( 0.08412497154685684431, 61.29016009911742202, 2.051811571683283653 ) ) ;
#3765 = CARTESIAN_POINT ( 'NONE',  ( -4.367998177332779619, 79.71679007096339831, -9.567661261929613303 ) ) ;
#3766 = DIRECTION ( 'NONE',  ( 0.5566703992264087075, 0.3213938048432681271, -0.7660444431189863401 ) ) ;
#3767 = DIRECTION ( 'NONE',  ( 0.8660254037844360431, 0.5000000000000045519, 4.336808689942049784E-16 ) ) ;
#3768 = ADVANCED_FACE ( 'NONE', ( #12344 ), #991, .T. ) ;
#3769 = CIRCLE ( 'NONE', #16641, 11.98469917212512215 ) ;
#3770 = LINE ( 'NONE', #278, #19793 ) ;
#3772 = ORIENTED_EDGE ( 'NONE', *, *, #14328, .F. ) ;
#3771 = ORIENTED_EDGE ( 'NONE', *, *, #1645, .F. ) ;
#3773 = ORIENTED_EDGE ( 'NONE', *, *, #14700, .F. ) ;
#3774 = LINE ( 'NONE', #13648, #6438 ) ;
#3776 = DIRECTION ( 'NONE',  ( -0.000000000000000000, 4.625929269271485914E-16, -1.000000000000000000 ) ) ;
#3775 = AXIS2_PLACEMENT_3D ( 'NONE', #19400, #17816, #11345 ) ;
#3777 = CIRCLE ( 'NONE', #8511, 12.47473710546057823 ) ;
#3778 = ORIENTED_EDGE ( 'NONE', *, *, #319, .F. ) ;
#3779 = CARTESIAN_POINT ( 'NONE',  ( 81.62020900107658861, 64.01414927466113625, 0.4645082096952444228 ) ) ;
#3780 = LINE ( 'NONE', #15051, #7804 ) ;
#3781 = CARTESIAN_POINT ( 'NONE',  ( 217.4773351563877384, 38.03360863815007775, -16.20791459969590065 ) ) ;
#3782 = EDGE_LOOP ( 'NONE', ( #6393, #4032, #4528, #3877 ) ) ;
#3783 = ADVANCED_FACE ( 'NONE', ( #4170 ), #12553, .T. ) ;
#3784 = CARTESIAN_POINT ( 'NONE',  ( -15.99999999999999289, 65.74999999999998579, 0.000000000000000000 ) ) ;
#3785 = EDGE_CURVE ( 'NONE', #7341, #6420, #785, .T. ) ;
#3786 = CARTESIAN_POINT ( 'NONE',  ( 208.6876230897591142, 11.60254374963070667, -25.63868392505628435 ) ) ;
#3787 = CIRCLE ( 'NONE', #9196, 13.99999999999999822 ) ;
#3788 = CARTESIAN_POINT ( 'NONE',  ( 85.37797649651368204, 230.0773763115391262, -28.99999999999998934 ) ) ;
#3789 = AXIS2_PLACEMENT_3D ( 'NONE', #18321, #3894, #15269 ) ;
#3790 = CYLINDRICAL_SURFACE ( 'NONE', #17013, 13.50000000000000711 ) ;
#3791 = CARTESIAN_POINT ( 'NONE',  ( -26.37630993324036766, 50.77084747640196127, -7.029141103310240446 ) ) ;
#3792 = CARTESIAN_POINT ( 'NONE',  ( -18.07496646850146149, 19.65148331647667845, 12.32752590463885412 ) ) ;
#3793 = PLANE ( 'NONE',  #15687 ) ;
#3794 = CARTESIAN_POINT ( 'NONE',  ( 215.2205796351215668, 15.55135787388338464, -18.06789442459603023 ) ) ;
#3795 = PRODUCT_DEFINITION ( 'UNKNOWN', '', #19579, #17430 ) ;
#3797 = ORIENTED_EDGE ( 'NONE', *, *, #6157, .F. ) ;
#3796 = VERTEX_POINT ( 'NONE', #17001 ) ;
#3798 = CARTESIAN_POINT ( 'NONE',  ( 62.27440062445415947, 78.36885602720158772, -12.89736757990179861 ) ) ;
#3799 = ORIENTED_EDGE ( 'NONE', *, *, #10826, .F. ) ;
#3800 = ORIENTED_EDGE ( 'NONE', *, *, #7974, .T. ) ;
#3801 = CARTESIAN_POINT ( 'NONE',  ( 215.1325240088992246, 19.62451685178295691, -15.47241223420017953 ) ) ;
#3802 = CARTESIAN_POINT ( 'NONE',  ( 217.4675698996929896, 9.683250065417357888, -20.66514661561436483 ) ) ;
#3803 = CIRCLE ( 'NONE', #101, 3.902363844300875240 ) ;
#3804 = EDGE_CURVE ( 'NONE', #3560, #5187, #18285, .T. ) ;
#3805 = ORIENTED_EDGE ( 'NONE', *, *, #13350, .T. ) ;
#3806 = ADVANCED_FACE ( 'NONE', ( #7436 ), #10494, .T. ) ;
#3807 = CARTESIAN_POINT ( 'NONE',  ( -15.99999999999999289, 9.999999999999994671, 0.000000000000000000 ) ) ;
#3808 = B_SPLINE_CURVE_WITH_KNOTS ( 'NONE', 3,
 ( #16729, #5676, #18736, #10447, #8868, #12165, #3999, #10560, #20003, #615, #17045, #2206, #19893, #18629, #8663, #8766, #11962, #4210, #13866, #10654 ),
 .UNSPECIFIED., .F., .F.,
 ( 4, 2, 2, 2, 2, 2, 2, 2, 2, 4 ),
 ( 0.008555345346386189487, 0.009089294358497951309, 0.009623243370609713132, 0.01069114139483322810, 0.01175903941905674134, 0.01282693744328025631, 0.01389483546750376781, 0.01496273349172728279, 0.01603063151595079602, 0.01709852954017430926 ),
 .UNSPECIFIED. ) ;
#3809 = DIRECTION ( 'NONE',  ( 0.000000000000000000, 0.000000000000000000, -1.000000000000000000 ) ) ;
#3810 = VERTEX_POINT ( 'NONE', #13932 ) ;
#3811 = MANIFOLD_SOLID_BREP ( 'Chamfer2', #17459 ) ;
#3812 = CARTESIAN_POINT ( 'NONE',  ( 217.5218984862054299, 37.95642268675135966, -13.56204498775453260 ) ) ;
#3813 = ADVANCED_FACE ( 'NONE', ( #15116 ), #12021, .T. ) ;
#3814 = ORIENTED_EDGE ( 'NONE', *, *, #18745, .T. ) ;
#3815 = CARTESIAN_POINT ( 'NONE',  ( -35.00000000000000000, 65.00000000000000000, -12.50000000000000000 ) ) ;
#3816 = CARTESIAN_POINT ( 'NONE',  ( 220.2180084519553134, 35.41797800104779270, -14.00000000000005507 ) ) ;
#3817 = FACE_OUTER_BOUND ( 'NONE', #15287, .T. ) ;
#3818 = AXIS2_PLACEMENT_3D ( 'NONE', #4217, #17051, #17151 ) ;
#3819 = VERTEX_POINT ( 'NONE', #18382 ) ;
#3820 = CARTESIAN_POINT ( 'NONE',  ( 5.000000000000000000, -2.342598717236899386, 4.057500000000001883 ) ) ;
#3821 = DIRECTION ( 'NONE',  ( 0.000000000000000000, 1.000000000000000000, -1.355657144061424088E-15 ) ) ;
#3822 = CARTESIAN_POINT ( 'NONE',  ( 226.7538876070129277, 41.96614847458961606, -11.35524774226743361 ) ) ;
#3823 = B_SPLINE_CURVE_WITH_KNOTS ( 'NONE', 3,
 ( #13080, #1426, #12980, #9455 ),
 .UNSPECIFIED., .F., .F.,
 ( 4, 4 ),
 ( 4.014844339177962562E-06, 0.0004560680861191103897 ),
 .UNSPECIFIED. ) ;
#3824 = ORIENTED_EDGE ( 'NONE', *, *, #13923, .F. ) ;
#3826 = ADVANCED_FACE ( 'NONE', ( #10296 ), #16787, .T. ) ;
#3825 = CARTESIAN_POINT ( 'NONE',  ( -4.701390418375630986, 65.75000000000000000, 5.347094680480811490 ) ) ;
#3827 = ORIENTED_EDGE ( 'NONE', *, *, #16546, .F. ) ;
#3828 = DIRECTION ( 'NONE',  ( 0.8660254037844360431, 0.5000000000000045519, 4.336808689942050277E-16 ) ) ;
#3829 = FACE_OUTER_BOUND ( 'NONE', #1692, .T. ) ;
#3830 = EDGE_CURVE ( 'NONE', #688, #1818, #13718, .T. ) ;
#3831 = ORIENTED_EDGE ( 'NONE', *, *, #4082, .F. ) ;
#3832 = CIRCLE ( 'NONE', #4525, 12.47473710546057823 ) ;
#3833 = DIRECTION ( 'NONE',  ( -0.000000000000000000, 0.000000000000000000, 1.000000000000000000 ) ) ;
#3834 = ORIENTED_EDGE ( 'NONE', *, *, #2637, .T. ) ;
#3835 = CARTESIAN_POINT ( 'NONE',  ( 76.02931450606715202, 53.32891420438221530, -18.26399853987619792 ) ) ;
#3836 = CARTESIAN_POINT ( 'NONE',  ( -25.88122819216030024, 79.85840876778742370, -10.43301765575532514 ) ) ;
#3837 = LINE ( 'NONE', #7012, #17778 ) ;
#3838 = LINE ( 'NONE', #10078, #5063 ) ;
#3839 = EDGE_CURVE ( 'NONE', #13750, #12912, #15329, .T. ) ;
#3840 = ORIENTED_EDGE ( 'NONE', *, *, #1283, .T. ) ;
#3841 = EDGE_CURVE ( 'NONE', #13156, #6779, #18587, .T. ) ;
#3842 = DIRECTION ( 'NONE',  ( 0.8296432542242749841, 0.4789947561577487245, -0.2868032327110942581 ) ) ;
#3843 = B_SPLINE_CURVE_WITH_KNOTS ( 'NONE', 3,
 ( #17939, #17837, #9951, #14564 ),
 .UNSPECIFIED., .F., .F.,
 ( 4, 4 ),
 ( 1.346298403970142578E-06, 0.0004533995401838951194 ),
 .UNSPECIFIED. ) ;
#3844 = DIRECTION ( 'NONE',  ( 0.5000000000000049960, -0.8660254037844358210, 0.000000000000000000 ) ) ;
#3845 = CARTESIAN_POINT ( 'NONE',  ( 208.2224579217690632, 4.087982952467670295, -25.92587471718749725 ) ) ;
#3846 = ORIENTED_EDGE ( 'NONE', *, *, #15147, .T. ) ;
#3847 = VECTOR ( 'NONE', #6152, 1000.000000000000114 ) ;
#3848 = AXIS2_PLACEMENT_3D ( 'NONE', #4030, #12321, #9309 ) ;
#3850 = EDGE_CURVE ( 'NONE', #11864, #18065, #20696, .T. ) ;
#3849 = FILL_AREA_STYLE ('',( #13823 ) ) ;
#3851 = CARTESIAN_POINT ( 'NONE',  ( 62.00490953756749946, 186.5607158131435028, 11.00000000000001066 ) ) ;
#3852 = DIRECTION ( 'NONE',  ( 0.5000000000000054401, -0.8660254037844354880, -1.665334536937734318E-16 ) ) ;
#3853 = FACE_OUTER_BOUND ( 'NONE', #4942, .T. ) ;
#3855 = ORIENTED_EDGE ( 'NONE', *, *, #9263, .T. ) ;
#3854 = ORIENTED_EDGE ( 'NONE', *, *, #5139, .T. ) ;
#3856 = ORIENTED_EDGE ( 'NONE', *, *, #6024, .T. ) ;
#3857 = CARTESIAN_POINT ( 'NONE',  ( 10.49211908931699178, -10.00000000000000000, 0.000000000000000000 ) ) ;
#3858 = CARTESIAN_POINT ( 'NONE',  ( 220.9434763298129951, 32.03007601957106232, -12.62147488791611671 ) ) ;
#3859 = CARTESIAN_POINT ( 'NONE',  ( 205.7420593526227890, 14.20292955466599238, -26.96550585544247269 ) ) ;
#3860 = EDGE_CURVE ( 'NONE', #6967, #13875, #6093, .T. ) ;
#3861 = DIRECTION ( 'NONE',  ( -0.8660254037844378194, -0.5000000000000013323, -0.000000000000000000 ) ) ;
#3862 = CARTESIAN_POINT ( 'NONE',  ( -25.99999999999999289, 4.999999999999994671, 7.500000000000009770 ) ) ;
#3863 = CARTESIAN_POINT ( 'NONE',  ( 198.4834855446717938, -1.277216147272815849, -16.79062062844341696 ) ) ;
#3864 = ORIENTED_EDGE ( 'NONE', *, *, #1632, .F. ) ;
#3865 = CARTESIAN_POINT ( 'NONE',  ( 80.87396291321206832, 53.74885471499349876, -21.51050425557589918 ) ) ;
#3866 = DIRECTION ( 'NONE',  ( 0.5000000000000054401, -0.8660254037844354880, 0.000000000000000000 ) ) ;
#3867 = ORIENTED_EDGE ( 'NONE', *, *, #12518, .F. ) ;
#3868 = CARTESIAN_POINT ( 'NONE',  ( -104.9618400369722622, 181.7992397999509819, 8.042028396309241600 ) ) ;
#3869 = CARTESIAN_POINT ( 'NONE',  ( 229.4690490064201356, 37.26335098006654079, -12.10162843130820143 ) ) ;
#3870 = CARTESIAN_POINT ( 'NONE',  ( 5.000000000000004441, -4.685197434473809430, 6.071532165918824830E-15 ) ) ;
#3871 = CARTESIAN_POINT ( 'NONE',  ( 28.00000000000001066, 64.25000000000000000, 75.00000000000000000 ) ) ;
#3872 = CARTESIAN_POINT ( 'NONE',  ( 98.63149783568741213, 199.9241707403680834, 8.516312532717298822 ) ) ;
#3873 = DIRECTION ( 'NONE',  ( -0.4084849465052256545, 0.7075166814741008503, 0.5766803221148600889 ) ) ;
#3875 = ORIENTED_EDGE ( 'NONE', *, *, #15962, .T. ) ;
#3874 = ORIENTED_EDGE ( 'NONE', *, *, #10282, .F. ) ;
#3876 = ORIENTED_EDGE ( 'NONE', *, *, #150, .F. ) ;
#3877 = ORIENTED_EDGE ( 'NONE', *, *, #992, .T. ) ;
#3878 = VECTOR ( 'NONE', #12139, 1000.000000000000114 ) ;
#3879 = DIRECTION ( 'NONE',  ( -0.5000000000000045519, 0.8660254037844360431, 3.469446951953612710E-16 ) ) ;
#3880 = CARTESIAN_POINT ( 'NONE',  ( 229.4896559907413689, 37.22765863623112637, -12.08027307405518869 ) ) ;
#3881 = ORIENTED_EDGE ( 'NONE', *, *, #19491, .F. ) ;
#3882 = VERTEX_POINT ( 'NONE', #4688 ) ;
#3883 = ORIENTED_EDGE ( 'NONE', *, *, #17795, .F. ) ;
#3884 = FILL_AREA_STYLE ('',( #7265 ) ) ;
#3885 = DIRECTION ( 'NONE',  ( 0.8660254037844363761, 0.5000000000000041078, 0.000000000000000000 ) ) ;
#3886 = FACE_OUTER_BOUND ( 'NONE', #7054, .T. ) ;
#3887 = ORIENTED_EDGE ( 'NONE', *, *, #4751, .T. ) ;
#3888 = CARTESIAN_POINT ( 'NONE',  ( 204.5209968812124544, 13.49794880809988484, -27.13030671846411579 ) ) ;
#3889 = LINE ( 'NONE', #10341, #13471 ) ;
#3890 = ORIENTED_EDGE ( 'NONE', *, *, #16305, .T. ) ;
#3891 = B_SPLINE_CURVE_WITH_KNOTS ( 'NONE', 3,
 ( #12947, #6760, #3284, #1698 ),
 .UNSPECIFIED., .F., .F.,
 ( 4, 4 ),
 ( 8.676057317371754181E-07, 0.0005667938280266552773 ),
 .UNSPECIFIED. ) ;
#3892 = CARTESIAN_POINT ( 'NONE',  ( 197.4890135470689643, -2.108974046597433816, -15.47241223419981715 ) ) ;
#3893 = AXIS2_PLACEMENT_3D ( 'NONE', #19737, #564, #5207 ) ;
#3894 = DIRECTION ( 'NONE',  ( 1.000000000000000000, 0.000000000000000000, 0.000000000000000000 ) ) ;
#3895 = CARTESIAN_POINT ( 'NONE',  ( -26.75428091535899000, 51.05733496925417825, -6.497914592029476744 ) ) ;
#3896 = CARTESIAN_POINT ( 'NONE',  ( 209.9028093415542173, 12.48114176340364700, -14.15605348658545282 ) ) ;
#3897 = CARTESIAN_POINT ( 'NONE',  ( 218.1659316888324724, 38.32692611279011885, -14.35673080489363862 ) ) ;
#3898 = CARTESIAN_POINT ( 'NONE',  ( 0.000000000000000000, 2.342598717236856309, 4.057500000000020535 ) ) ;
#3899 = EDGE_CURVE ( 'NONE', #9907, #19392, #12200, .T. ) ;
#3901 = VERTEX_POINT ( 'NONE', #1309 ) ;
#3900 = VERTEX_POINT ( 'NONE', #9444 ) ;
#3902 = CARTESIAN_POINT ( 'NONE',  ( 58.80800210575738163, 85.32167585634152829, -14.25381645728047708 ) ) ;
#3903 = ORIENTED_EDGE ( 'NONE', *, *, #2767, .F. ) ;
#3904 = ORIENTED_EDGE ( 'NONE', *, *, #18283, .T. ) ;
#3905 = ORIENTED_EDGE ( 'NONE', *, *, #8879, .F. ) ;
#3906 = ORIENTED_EDGE ( 'NONE', *, *, #1187, .T. ) ;
#3907 = CARTESIAN_POINT ( 'NONE',  ( 199.2144802262915846, 21.04890371929339921, -14.00000000000005507 ) ) ;
#3908 = AXIS2_PLACEMENT_3D ( 'NONE', #6957, #13552, #18208 ) ;
#3909 = CARTESIAN_POINT ( 'NONE',  ( 200.1138010445123143, -0.5935522783828972582, -22.49869731917958404 ) ) ;
#3910 = CIRCLE ( 'NONE', #9655, 13.99999999999999822 ) ;
#3911 = VERTEX_POINT ( 'NONE', #9338 ) ;
#3912 = CARTESIAN_POINT ( 'NONE',  ( 216.1231765438266166, 15.71844586073754790, -16.84511136304323387 ) ) ;
#3913 = ORIENTED_EDGE ( 'NONE', *, *, #5748, .T. ) ;
#3914 = AXIS2_PLACEMENT_3D ( 'NONE', #15936, #4983, #4679 ) ;
#3916 = EDGE_CURVE ( 'NONE', #4803, #10151, #12448, .T. ) ;
#3915 = DIRECTION ( 'NONE',  ( -0.2597919750177127840, 0.4499729001293399921, -0.8544194045464951204 ) ) ;
#3917 = CARTESIAN_POINT ( 'NONE',  ( 0.000000000000000000, -10.00000000000000000, 0.000000000000000000 ) ) ;
#3918 = CARTESIAN_POINT ( 'NONE',  ( 218.2325500505156413, 38.65091476268579385, -13.96598824437076836 ) ) ;
#3919 = FACE_OUTER_BOUND ( 'NONE', #10657, .T. ) ;
#3920 = DIRECTION ( 'NONE',  ( 0.000000000000000000, -1.000000000000000000, 0.000000000000000000 ) ) ;
#3921 = DIRECTION ( 'NONE',  ( -0.5000000000000061062, 0.000000000000000000, 0.8660254037844351549 ) ) ;
#3922 = AXIS2_PLACEMENT_3D ( 'NONE', #2521, #4523, #14297 ) ;
#3923 = EDGE_CURVE ( 'NONE', #19176, #9963, #4379, .T. ) ;
#3924 = ORIENTED_EDGE ( 'NONE', *, *, #2788, .F. ) ;
#3925 = CARTESIAN_POINT ( 'NONE',  ( 215.8800731390675764, 9.281929250168950318, -4.915515517929356371 ) ) ;
#3926 = FACE_OUTER_BOUND ( 'NONE', #15077, .T. ) ;
#3927 = LINE ( 'NONE', #8806, #11231 ) ;
#3928 = AXIS2_PLACEMENT_3D ( 'NONE', #9114, #12328, #18784 ) ;
#3929 = ADVANCED_FACE ( 'NONE', ( #18908 ), #1031, .T. ) ;
#3930 = EDGE_LOOP ( 'NONE', ( #10670, #19011, #15236, #8625, #528, #8180 ) ) ;
#3931 = CIRCLE ( 'NONE', #4270, 5.000000000000035527 ) ;
#3932 = B_SPLINE_CURVE_WITH_KNOTS ( 'NONE', 3,
 ( #5184, #7096, #538, #6663 ),
 .UNSPECIFIED., .F., .F.,
 ( 4, 4 ),
 ( 4.014081919340420194E-07, 0.0004524546499717620966 ),
 .UNSPECIFIED. ) ;
#3933 = CARTESIAN_POINT ( 'NONE',  ( 82.14679489777772403, 61.41165722483968636, -0.0001489139912725718411 ) ) ;
#3934 = EDGE_LOOP ( 'NONE', ( #4702, #19824, #7717, #12186 ) ) ;
#3935 = DIRECTION ( 'NONE',  ( 0.8660254037844355990, 0.5000000000000054401, -3.198355172551227375E-14 ) ) ;
#3936 = CARTESIAN_POINT ( 'NONE',  ( 213.7787453705537075, 18.84291239051101741, -11.24974199967302013 ) ) ;
#3937 = EDGE_CURVE ( 'NONE', #18465, #13223, #17962, .T. ) ;
#3938 = CARTESIAN_POINT ( 'NONE',  ( -15.99999999999999289, 15.09941697557068352, 33.65884678261294027 ) ) ;
#3939 = AXIS2_PLACEMENT_3D ( 'NONE', #13181, #18468, #3723 ) ;
#3940 = DIRECTION ( 'NONE',  ( 2.052623352751953829E-17, -1.550730178515671504E-16, -1.000000000000000000 ) ) ;
#3941 = VERTEX_POINT ( 'NONE', #6167 ) ;
#3942 = CONICAL_SURFACE ( 'NONE', #9682, 10.85470691220533190, 0.8171114040043576665 ) ;
#3943 = CARTESIAN_POINT ( 'NONE',  ( 81.73281949542425195, 63.23532430020726025, -25.38086878997933837 ) ) ;
#3944 = CARTESIAN_POINT ( 'NONE',  ( -24.90922013266621704, 80.00000000007942447, -8.779353540718402016 ) ) ;
#3945 = CARTESIAN_POINT ( 'NONE',  ( 200.4559313511114453, 7.026984212619883152, -3.762296834228767928 ) ) ;
#3946 = CARTESIAN_POINT ( 'NONE',  ( 5.000000000000000000, 2.342598717236913153, 4.057499999999995666 ) ) ;
#3947 = ADVANCED_FACE ( 'NONE', ( #15741 ), #12656, .F. ) ;
#3948 = EDGE_LOOP ( 'NONE', ( #1103, #12176, #13988, #2172 ) ) ;
#3949 = DIRECTION ( 'NONE',  ( 0.000000000000000000, 0.000000000000000000, -1.000000000000000000 ) ) ;
#3950 = EDGE_CURVE ( 'NONE', #18175, #8243, #20890, .T. ) ;
#3951 = SHAPE_REPRESENTATION ( 'Base Lock Knob', ( #18233 ), #6025 ) ;
#3952 = CARTESIAN_POINT ( 'NONE',  ( 210.5718816476998256, 5.444423373074280370, -2.341985411377013548 ) ) ;
#3953 = DIRECTION ( 'NONE',  ( 6.608470384673549052E-16, -1.000000000000000000, 0.000000000000000000 ) ) ;
#3954 = VERTEX_POINT ( 'NONE', #15942 ) ;
#3955 = DIRECTION ( 'NONE',  ( -0.5000000000000049960, 0.8660254037844357100, -0.000000000000000000 ) ) ;
#3956 = DIRECTION ( 'NONE',  ( 0.8660254037844380415, 0.5000000000000008882, 0.000000000000000000 ) ) ;
#3957 = CIRCLE ( 'NONE', #9361, 5.000000000000008882 ) ;
#3958 = DIRECTION ( 'NONE',  ( 0.8660254037844380415, 0.5000000000000014433, 0.000000000000000000 ) ) ;
#3959 = DIRECTION ( 'NONE',  ( -0.8660254037844370423, -0.5000000000000027756, 0.000000000000000000 ) ) ;
#3960 = ADVANCED_FACE ( 'NONE', ( #12861, #1416, #17739, #9131, #19217 ), #14467, .F. ) ;
#3961 = ORIENTED_EDGE ( 'NONE', *, *, #8809, .F. ) ;
#3962 = VERTEX_POINT ( 'NONE', #6057 ) ;
#3963 = VERTEX_POINT ( 'NONE', #6262 ) ;
#3964 = ADVANCED_FACE ( 'NONE', ( #19315 ), #12755, .F. ) ;
#3965 = DIRECTION ( 'NONE',  ( 0.5000000000000054401, -0.8660254037844354880, 0.000000000000000000 ) ) ;
#3966 = LINE ( 'NONE', #20282, #15990 ) ;
#3967 = CARTESIAN_POINT ( 'NONE',  ( -15.99999999999999289, 9.999999999999994671, 0.000000000000000000 ) ) ;
#3968 = CARTESIAN_POINT ( 'NONE',  ( 206.2818991689553627, 10.21359839635873357, -26.12768996730768478 ) ) ;
#3969 = CARTESIAN_POINT ( 'NONE',  ( -30.00000000000019895, 4.999999999999801048, -0.4747169640371201038 ) ) ;
#3970 = B_SPLINE_CURVE_WITH_KNOTS ( 'NONE', 3,
 ( #11157, #17742, #3112, #3206 ),
 .UNSPECIFIED., .F., .F.,
 ( 4, 4 ),
 ( 2.845336965351252746E-07, 0.0004523377754764257254 ),
 .UNSPECIFIED. ) ;
#3971 = CARTESIAN_POINT ( 'NONE',  ( 0.000000000000000000, 4.685197434473812983, -6.938893903907228378E-15 ) ) ;
#3972 = EDGE_CURVE ( 'NONE', #17245, #11939, #11865, .T. ) ;
#3973 = VERTEX_POINT ( 'NONE', #17630 ) ;
#3974 = CIRCLE ( 'NONE', #11089, 15.00000000000000000 ) ;
#3975 = CARTESIAN_POINT ( 'NONE',  ( 80.79037351930210775, 57.71461494556285743, -23.29247368251557759 ) ) ;
#3976 = CARTESIAN_POINT ( 'NONE',  ( 207.8527399996651184, 15.42153159440924881, -3.125199447383529172 ) ) ;
#3977 = VECTOR ( 'NONE', #12881, 1000.000000000000000 ) ;
#3978 = ORIENTED_EDGE ( 'NONE', *, *, #5974, .T. ) ;
#3979 = CARTESIAN_POINT ( 'NONE',  ( 205.0662616026534693, 10.91332106064940888, -14.00000000000005507 ) ) ;
#3980 = DIRECTION ( 'NONE',  ( 0.000000000000000000, 0.000000000000000000, 1.000000000000000000 ) ) ;
#3981 = EDGE_CURVE ( 'NONE', #6334, #17905, #20928, .T. ) ;
#3982 = CARTESIAN_POINT ( 'NONE',  ( 54.01452848080093361, 170.4004617752990498, -29.00000000000000000 ) ) ;
#3983 = DIRECTION ( 'NONE',  ( -0.8660254037844360431, -0.5000000000000044409, -4.336808689942049290E-16 ) ) ;
#3984 = DIRECTION ( 'NONE',  ( -0.8660254037844361541, -0.5000000000000042188, 6.872020471724001723E-17 ) ) ;
#3986 = EDGE_LOOP ( 'NONE', ( #1468, #20086, #13542, #19228 ) ) ;
#3985 = EDGE_LOOP ( 'NONE', ( #13017, #20791, #3373, #8611 ) ) ;
#3987 = ORIENTED_EDGE ( 'NONE', *, *, #7695, .F. ) ;
#3988 = CARTESIAN_POINT ( 'NONE',  ( 85.37797649651368204, 230.0773763115391262, -28.99999999999998934 ) ) ;
#3989 = PLANE ( 'NONE',  #367 ) ;
#3990 = EDGE_CURVE ( 'NONE', #600, #7107, #3109, .T. ) ;
#3991 = ORIENTED_EDGE ( 'NONE', *, *, #7346, .T. ) ;
#3992 = B_SPLINE_CURVE_WITH_KNOTS ( 'NONE', 3,
 ( #3145, #4725, #7900, #20625 ),
 .UNSPECIFIED., .F., .F.,
 ( 4, 4 ),
 ( 6.424236652724635136E-05, 0.0007368931585819213240 ),
 .UNSPECIFIED. ) ;
#3993 = AXIS2_PLACEMENT_3D ( 'NONE', #7668, #19029, #4505 ) ;
#3994 = PRODUCT_DEFINITION_SHAPE ( 'NONE', 'NONE',  #20950 ) ;
#3995 = CARTESIAN_POINT ( 'NONE',  ( 226.7369255887865904, 41.99552755195625764, -11.32356490392471393 ) ) ;
#3996 = CARTESIAN_POINT ( 'NONE',  ( 195.4998201364199417, 4.165572068683992768, -11.22353489230383339 ) ) ;
#3997 = AXIS2_PLACEMENT_3D ( 'NONE', #9336, #18906, #1307 ) ;
#3998 = CARTESIAN_POINT ( 'NONE',  ( 104.7973891242897650, 32.44196698708787352, -12.50000000000000000 ) ) ;
#3999 = CARTESIAN_POINT ( 'NONE',  ( -17.72229213209295651, 71.26752244718856844, -4.704935945893314653 ) ) ;
#4000 = CARTESIAN_POINT ( 'NONE',  ( 221.6709703790052117, 32.25350094652943511, -13.17988343266938145 ) ) ;
#4001 = CIRCLE ( 'NONE', #17892, 11.94520687646042667 ) ;
#4002 = LINE ( 'NONE', #18212, #14326 ) ;
#4003 = CARTESIAN_POINT ( 'NONE',  ( -29.51915980583113353, 50.03287237322234660, -11.46702022756807970 ) ) ;
#4004 = LINE ( 'NONE', #5792, #2138 ) ;
#4005 = FACE_OUTER_BOUND ( 'NONE', #18195, .T. ) ;
#4006 = CARTESIAN_POINT ( 'NONE',  ( -28.07387375345178882, 54.51268698003941893, 3.249670041809122889 ) ) ;
#4008 = ORIENTED_EDGE ( 'NONE', *, *, #12277, .F. ) ;
#4007 = ORIENTED_EDGE ( 'NONE', *, *, #9229, .T. ) ;
#4009 = CARTESIAN_POINT ( 'NONE',  ( 202.1874421558074744, 25.46507160306319406, -12.54005369788149693 ) ) ;
#4010 = CARTESIAN_POINT ( 'NONE',  ( 62.57915299879362436, 78.18516598039407484, -15.53707111529713636 ) ) ;
#4011 = EDGE_LOOP ( 'NONE', ( #7091, #9421, #18763, #7287 ) ) ;
#4012 = VERTEX_POINT ( 'NONE', #18044 ) ;
#4013 = ORIENTED_EDGE ( 'NONE', *, *, #19159, .F. ) ;
#4014 = LINE ( 'NONE', #12182, #4765 ) ;
#4015 = DIRECTION ( 'NONE',  ( 0.5000000000000041078, -0.8660254037844363761, 0.000000000000000000 ) ) ;
#4016 = EDGE_LOOP ( 'NONE', ( #13423, #14880 ) ) ;
#4017 = ORIENTED_EDGE ( 'NONE', *, *, #14339, .F. ) ;
#4018 = PLANE ( 'NONE',  #2284 ) ;
#4019 = EDGE_LOOP ( 'NONE', ( #15572, #16200, #3277, #15121, #17057 ) ) ;
#4020 = LINE ( 'NONE', #1063, #958 ) ;
#4021 = CARTESIAN_POINT ( 'NONE',  ( 219.3925639124447287, 34.71633512454243231, -17.56803216753791475 ) ) ;
#4022 = EDGE_CURVE ( 'NONE', #17056, #4395, #3259, .T. ) ;
#4023 = CARTESIAN_POINT ( 'NONE',  ( -12.94355555882016162, 19.06978034970748226, 12.12372807873016711 ) ) ;
#4025 = ORIENTED_EDGE ( 'NONE', *, *, #1948, .T. ) ;
#4024 = B_SPLINE_CURVE_WITH_KNOTS ( 'NONE', 3,
 ( #9191, #10898, #2956, #17376 ),
 .UNSPECIFIED., .F., .F.,
 ( 4, 4 ),
 ( 3.169130416727337534E-07, 0.0005858052687812763219 ),
 .UNSPECIFIED. ) ;
#4026 = CARTESIAN_POINT ( 'NONE',  ( 219.9164680944309396, 33.80890646304445113, -10.64970491435236255 ) ) ;
#4027 = CARTESIAN_POINT ( 'NONE',  ( 229.7285650908456205, 36.81385593646026422, -13.56204498775466583 ) ) ;
#4028 = CARTESIAN_POINT ( 'NONE',  ( 73.36131599811851345, 198.8908428320658288, 11.00000000000001066 ) ) ;
#4029 = DIRECTION ( 'NONE',  ( 0.8660254037844352659, 0.5000000000000056621, 0.000000000000000000 ) ) ;
#4030 = CARTESIAN_POINT ( 'NONE',  ( 209.3577037357181894, 3.480325248439694263, -14.00000000000005507 ) ) ;
#4031 = CARTESIAN_POINT ( 'NONE',  ( 201.5598379337182848, 7.133275713455735634, -25.46066938576250394 ) ) ;
#4032 = ORIENTED_EDGE ( 'NONE', *, *, #1741, .F. ) ;
#4033 = CARTESIAN_POINT ( 'NONE',  ( 81.70299675858660748, 56.27235011262846598, -1.678517931375763883 ) ) ;
#4034 = EDGE_CURVE ( 'NONE', #10335, #19279, #17840, .T. ) ;
#4035 = ORIENTED_EDGE ( 'NONE', *, *, #16531, .F. ) ;
#4036 = DIRECTION ( 'NONE',  ( -0.8660254037844355990, -0.5000000000000055511, 0.000000000000000000 ) ) ;
#4037 = DIRECTION ( 'NONE',  ( 0.000000000000000000, -1.110768649713242108E-15, -1.000000000000000000 ) ) ;
#4038 = EDGE_CURVE ( 'NONE', #15921, #5032, #3512, .T. ) ;
#4039 = DIRECTION ( 'NONE',  ( 0.9885408208161388099, 0.000000000000000000, 0.1509537862398780406 ) ) ;
#4040 = VECTOR ( 'NONE', #19153, 1000.000000000000000 ) ;
#4041 = ORIENTED_EDGE ( 'NONE', *, *, #945, .T. ) ;
#4042 = CARTESIAN_POINT ( 'NONE',  ( 81.17621279504307097, 64.86352945118836999, -25.50000000000000355 ) ) ;
#4043 = EDGE_CURVE ( 'NONE', #10411, #18303, #14990, .T. ) ;
#4044 = DIRECTION ( 'NONE',  ( -0.3155439721630312055, 0.5465381918084659674, 0.7757112907044145800 ) ) ;
#4045 = CARTESIAN_POINT ( 'NONE',  ( 205.8264633344831225, 9.596613037118636669, -14.00000000000005507 ) ) ;
#4046 = CARTESIAN_POINT ( 'NONE',  ( 58.37797649651341203, 276.8427481158987007, -0.9999999999999826805 ) ) ;
#4047 = EDGE_LOOP ( 'NONE', ( #20065, #4159, #14350 ) ) ;
#4048 = VECTOR ( 'NONE', #7803, 1000.000000000000227 ) ;
#4049 = CARTESIAN_POINT ( 'NONE',  ( 127.2868417743716094, 73.48909236273162549, -8.999999999999934275 ) ) ;
#4050 = B_SPLINE_CURVE_WITH_KNOTS ( 'NONE', 3,
 ( #5422, #18383, #18588, #10514 ),
 .UNSPECIFIED., .F., .F.,
 ( 4, 4 ),
 ( 6.863716774068141194E-05, 0.0007412879597948096892 ),
 .UNSPECIFIED. ) ;
#4051 = CIRCLE ( 'NONE', #19949, 5.000000000000000888 ) ;
#4052 = CARTESIAN_POINT ( 'NONE',  ( 82.49529059433407951, 181.0703347563770365, 16.00000000000001066 ) ) ;
#4053 = CARTESIAN_POINT ( 'NONE',  ( 5.000000000000004441, 0.000000000000000000, 0.000000000000000000 ) ) ;
#4054 = ORIENTED_EDGE ( 'NONE', *, *, #3688, .T. ) ;
#4055 = DIRECTION ( 'NONE',  ( 0.4999999999999995004, -0.8660254037844390407, 0.000000000000000000 ) ) ;
#4056 = CARTESIAN_POINT ( 'NONE',  ( 208.0983737146324870, 5.661548828456886895, -14.00000000000005507 ) ) ;
#4057 = PRODUCT_RELATED_PRODUCT_CATEGORY ( 'part', '', ( #10591 ) ) ;
#4058 = DIRECTION ( 'NONE',  ( -0.4999999999999995004, 0.8660254037844390407, 0.000000000000000000 ) ) ;
#4059 = CARTESIAN_POINT ( 'NONE',  ( 28.51452848080068847, 214.5677573683055357, -19.00000000000000000 ) ) ;
#4060 = EDGE_CURVE ( 'NONE', #884, #951, #4429, .T. ) ;
#4062 = ORIENTED_EDGE ( 'NONE', *, *, #3059, .F. ) ;
#4061 = EDGE_LOOP ( 'NONE', ( #15149, #11924, #7442, #12458, #14665 ) ) ;
#4063 = AXIS2_PLACEMENT_3D ( 'NONE', #11056, #9339, #886 ) ;
#4064 = VERTEX_POINT ( 'NONE', #5192 ) ;
#4065 = CARTESIAN_POINT ( 'NONE',  ( 35.31538279416584913, 262.7883321626826501, 8.042028396309257587 ) ) ;
#4066 = CARTESIAN_POINT ( 'NONE',  ( 201.5199827852405861, 7.641314594545947969, -24.85758746085086557 ) ) ;
#4067 = EDGE_LOOP ( 'NONE', ( #5245, #6014, #15021, #5942 ) ) ;
#4068 = CARTESIAN_POINT ( 'NONE',  ( -33.07648103134474837, 77.63984378200004244, -4.412136689679511115 ) ) ;
#4069 = B_SPLINE_CURVE_WITH_KNOTS ( 'NONE', 3,
 ( #15194, #17181, #11996, #18454 ),
 .UNSPECIFIED., .F., .F.,
 ( 4, 4 ),
 ( 5.972954429729013304E-06, 0.0003733324143565315990 ),
 .UNSPECIFIED. ) ;
#4070 = EDGE_CURVE ( 'NONE', #688, #14131, #1717, .T. ) ;
#4071 = CARTESIAN_POINT ( 'NONE',  ( -29.99999999999999645, -10.00000000000000000, -15.00000000000000000 ) ) ;
#4072 = CARTESIAN_POINT ( 'NONE',  ( -28.48162945689469083, 6.472597147970983400, -0.7888061438404905257 ) ) ;
#4073 = CARTESIAN_POINT ( 'NONE',  ( 5.000000000000000000, 4.685197434473812983, -6.938893903907228378E-15 ) ) ;
#4075 = ADVANCED_FACE ( 'NONE', ( #8378 ), #449, .T. ) ;
#4074 = AXIS2_PLACEMENT_3D ( 'NONE', #594, #16811, #16491 ) ;
#4076 = ORIENTED_EDGE ( 'NONE', *, *, #19588, .F. ) ;
#4077 = VERTEX_POINT ( 'NONE', #16446 ) ;
#4078 = CARTESIAN_POINT ( 'NONE',  ( 81.37385535124417402, 59.06361191445762415, -24.08546180346211685 ) ) ;
#4079=STYLED_ITEM('',(#20988),#3700);
#4080 = LINE ( 'NONE', #8948, #3233 ) ;
#4081 = AXIS2_PLACEMENT_3D ( 'NONE', #19989, #15461, #2621 ) ;
#4082 = EDGE_CURVE ( 'NONE', #3117, #5485, #13375, .T. ) ;
#4083 = EDGE_LOOP ( 'NONE', ( #14996, #1298, #1256, #6821, #6211, #6184 ) ) ;
#4084 = CYLINDRICAL_SURFACE ( 'NONE', #4074, 12.99999999999999822 ) ;
#4085 = CARTESIAN_POINT ( 'NONE',  ( 218.4367820612134494, 37.88530424025100984, -12.10162843130809840 ) ) ;
#4086 = AXIS2_PLACEMENT_3D ( 'NONE', #8680, #632, #10143 ) ;
#4087 = CARTESIAN_POINT ( 'NONE',  ( -34.66668267600675080, 64.25000000000000000, 1.813692929321156333 ) ) ;
#4088 = DIRECTION ( 'NONE',  ( -0.000000000000000000, 1.000000000000000000, -0.000000000000000000 ) ) ;
#4089 = DIRECTION ( 'NONE',  ( -1.000000000000000000, 0.000000000000000000, 0.000000000000000000 ) ) ;
#4090 = ORIENTED_EDGE ( 'NONE', *, *, #455, .T. ) ;
#4091 = ORIENTED_EDGE ( 'NONE', *, *, #6121, .F. ) ;
#4092 = CARTESIAN_POINT ( 'NONE',  ( 221.6773453713352353, 32.27248394197634696, -14.91677899116122319 ) ) ;
#4093 = DIRECTION ( 'NONE',  ( 0.000000000000000000, 0.000000000000000000, -1.000000000000000000 ) ) ;
#4094 = ADVANCED_FACE ( 'NONE', ( #4896, #9659 ), #336, .T. ) ;
#4095 = VECTOR ( 'NONE', #6838, 1000.000000000000227 ) ;
#4096 = VECTOR ( 'NONE', #20511, 1000.000000000000227 ) ;
#4097 = ORIENTED_EDGE ( 'NONE', *, *, #12346, .F. ) ;
#4098 = CARTESIAN_POINT ( 'NONE',  ( 0.000000000000000000, -1.759474945355379072, 3.047500000000001652 ) ) ;
#4099 = CYLINDRICAL_SURFACE ( 'NONE', #15307, 5.000000000000000888 ) ;
#4100 = AXIS2_PLACEMENT_3D ( 'NONE', #17999, #3251, #1464 ) ;
#4101 = CARTESIAN_POINT ( 'NONE',  ( 218.3216332057867248, 38.08474790828346102, -15.46846178913018477 ) ) ;
#4102 = ADVANCED_FACE ( 'NONE', ( #4988 ), #1823, .F. ) ;
#4103 = VECTOR ( 'NONE', #3879, 1000.000000000000227 ) ;
#4104 = FACE_BOUND ( 'NONE', #18020, .T. ) ;
#4105 = CARTESIAN_POINT ( 'NONE',  ( 203.2663706161054620, 1.741790851292542408, -3.346771071759890859 ) ) ;
#4106 = EDGE_CURVE ( 'NONE', #20359, #14752, #9812, .T. ) ;
#4107 = DIRECTION ( 'NONE',  ( -0.5000000000000051070, 0.8660254037844359321, -0.000000000000000000 ) ) ;
#4108 = ADVANCED_FACE ( 'NONE', ( #11466 ), #9151, .T. ) ;
#4109 = AXIS2_PLACEMENT_3D ( 'NONE', #14395, #6395, #6197 ) ;
#4110 = EDGE_CURVE ( 'NONE', #16764, #9609, #6894, .T. ) ;
#4111 = DIRECTION ( 'NONE',  ( 0.000000000000000000, 0.000000000000000000, 1.000000000000000000 ) ) ;
#4112 = CARTESIAN_POINT ( 'NONE',  ( -23.47727273277572380, 50.20802583047444756, -15.01355377214448517 ) ) ;
#4113 = PLANE ( 'NONE',  #19394 ) ;
#4114 = VECTOR ( 'NONE', #580, 1000.000000000000000 ) ;
#4115 = CARTESIAN_POINT ( 'NONE',  ( 205.8264633344831225, 9.596613037118636669, -14.00000000000005507 ) ) ;
#4116 = AXIS2_PLACEMENT_3D ( 'NONE', #7783, #14288, #12685 ) ;
#4117 = CARTESIAN_POINT ( 'NONE',  ( -27.66274264245146242, 58.14439702606364335, 4.503690111865336299 ) ) ;
#4119 = ORIENTED_EDGE ( 'NONE', *, *, #2027, .T. ) ;
#4118 = ORIENTED_EDGE ( 'NONE', *, *, #3198, .F. ) ;
#4120 = FACE_OUTER_BOUND ( 'NONE', #7915, .T. ) ;
#4121 = CARTESIAN_POINT ( 'NONE',  ( 62.43702563953799967, 78.27403789581164517, -12.60076481416450989 ) ) ;
#4122 = CIRCLE ( 'NONE', #12588, 8.000000000000000000 ) ;
#4123 = ADVANCED_FACE ( 'NONE', ( #6467 ), #18659, .T. ) ;
#4124 = VERTEX_POINT ( 'NONE', #14780 ) ;
#4125 = ORIENTED_EDGE ( 'NONE', *, *, #15707, .T. ) ;
#4126 = CARTESIAN_POINT ( 'NONE',  ( 227.4169190649082850, 40.49127522653217426, -17.62796654520765927 ) ) ;
#4127 = CARTESIAN_POINT ( 'NONE',  ( 0.4725499000616883993, 50.80107947907877985, -7.614411031363864879 ) ) ;
#4128 = LINE ( 'NONE', #20027, #5591 ) ;
#4129 = ORIENTED_EDGE ( 'NONE', *, *, #10460, .F. ) ;
#4130 = ORIENTED_EDGE ( 'NONE', *, *, #2416, .T. ) ;
#4131 = LINE ( 'NONE', #15182, #12779 ) ;
#4132 = EDGE_CURVE ( 'NONE', #9807, #5527, #6674, .T. ) ;
#4133 = AXIS2_PLACEMENT_3D ( 'NONE', #4396, #18716, #4295 ) ;
#4134 = CARTESIAN_POINT ( 'NONE',  ( 159.9952905943348469, 46.83639716978957068, 0.9999999999999386047 ) ) ;
#4135 = VECTOR ( 'NONE', #1377, 1000.000000000000227 ) ;
#4136 = DIRECTION ( 'NONE',  ( -0.000000000000000000, 1.000000000000000000, -0.000000000000000000 ) ) ;
#4137 = CARTESIAN_POINT ( 'NONE',  ( -15.34316709825168168, 20.06719728497707678, 12.48700296046530411 ) ) ;
#4138 = CONICAL_SURFACE ( 'NONE', #12604, 10.26794919243114634, 1.047197551196596965 ) ;
#4139 = DIRECTION ( 'NONE',  ( 0.000000000000000000, -0.9557539690135802291, 0.2941672155675891243 ) ) ;
#4140 = CARTESIAN_POINT ( 'NONE',  ( -27.95542020482363199, 74.48392764733534932, 3.658293529343086270 ) ) ;
#4141 = CARTESIAN_POINT ( 'NONE',  ( -20.99999999999998934, 15.09941697557068530, 0.9999999999999991118 ) ) ;
#4142 = EDGE_LOOP ( 'NONE', ( #14421, #653, #5770, #12835 ) ) ;
#4143 = CARTESIAN_POINT ( 'NONE',  ( -32.77872921741722223, 72.29984585682672105, 0.6063817381316165545 ) ) ;
#4144 = CARTESIAN_POINT ( 'NONE',  ( -20.31374355284814825, 65.74999999999995737, -2.528164662410434804 ) ) ;
#4145 = CARTESIAN_POINT ( 'NONE',  ( 221.4811267571203359, 32.81826275199232867, -11.70804666182404219 ) ) ;
#4146 = ORIENTED_EDGE ( 'NONE', *, *, #16467, .F. ) ;
#4147 = CIRCLE ( 'NONE', #17315, 4.999999999999977796 ) ;
#4148 = VECTOR ( 'NONE', #2557, 1000.000000000000227 ) ;
#4149 = CARTESIAN_POINT ( 'NONE',  ( 82.15152675072569366, 57.78258148490818513, -0.9124300798289324277 ) ) ;
#4150 = VECTOR ( 'NONE', #9927, 1000.000000000000000 ) ;
#4151 = VERTEX_POINT ( 'NONE', #8483 ) ;
#4152 = EDGE_CURVE ( 'NONE', #18151, #18856, #3408, .T. ) ;
#4153 = ORIENTED_EDGE ( 'NONE', *, *, #18186, .T. ) ;
#4154 = CARTESIAN_POINT ( 'NONE',  ( 8.000000000000000000, 7.960204194457795477E-16, -6.500000000000000000 ) ) ;
#4155 = CARTESIAN_POINT ( 'NONE',  ( 58.37797649651341203, 276.8427481158987007, 1.000000000000017097 ) ) ;
#4156 = SHAPE_DEFINITION_REPRESENTATION ( #12313, #4634 ) ;
#4157 = LINE ( 'NONE', #7641, #4865 ) ;
#4158 = VERTEX_POINT ( 'NONE', #11893 ) ;
#4159 = ORIENTED_EDGE ( 'NONE', *, *, #3215, .T. ) ;
#4160 = LINE ( 'NONE', #2581, #1648 ) ;
#4161 = AXIS2_PLACEMENT_3D ( 'NONE', #6643, #7491, #14088 ) ;
#4162 = PLANE ( 'NONE',  #1199 ) ;
#4163 = DIRECTION ( 'NONE',  ( -0.4439426092011872771, 0.7689311547811458203, -0.4600650377311618078 ) ) ;
#4164 = ADVANCED_FACE ( 'NONE', ( #12000 ), #13800, .T. ) ;
#4165 = CARTESIAN_POINT ( 'NONE',  ( 219.5521249847671186, 36.57132199813789697, -10.33191597617938484 ) ) ;
#4166 = CARTESIAN_POINT ( 'NONE',  ( 226.7820310402353243, 41.26444348584627875, -17.36588157897871909 ) ) ;
#4167 = DIRECTION ( 'NONE',  ( 0.3535533905932772836, -0.6123724356957930270, -0.7071067811865470176 ) ) ;
#4168 = PRODUCT_DEFINITION_SHAPE ( 'NONE', 'NONE',  #20956 ) ;
#4169 = VERTEX_POINT ( 'NONE', #18359 ) ;
#4170 = FACE_OUTER_BOUND ( 'NONE', #3035, .T. ) ;
#4171 = CARTESIAN_POINT ( 'NONE',  ( -4.044579795176349357, 74.48392764733533511, 3.658293529343076500 ) ) ;
#4172 = EDGE_CURVE ( 'NONE', #16360, #1288, #7532, .T. ) ;
#4173 = DIRECTION ( 'NONE',  ( -0.8660254037844354880, -0.5000000000000055511, 0.000000000000000000 ) ) ;
#4174 = FACE_OUTER_BOUND ( 'NONE', #4016, .T. ) ;
#4175 = VECTOR ( 'NONE', #6256, 1000.000000000000114 ) ;
#4177 = VERTEX_POINT ( 'NONE', #10273 ) ;
#4176 = ORIENTED_EDGE ( 'NONE', *, *, #12806, .T. ) ;
#4178 = ORIENTED_EDGE ( 'NONE', *, *, #9549, .F. ) ;
#4179 = ORIENTED_EDGE ( 'NONE', *, *, #16223, .T. ) ;
#4180 = FACE_OUTER_BOUND ( 'NONE', #1979, .T. ) ;
#4181 = CARTESIAN_POINT ( 'NONE',  ( 4.000000000000000000, -1.759474945355379072, 3.047500000000001652 ) ) ;
#4182 = VERTEX_POINT ( 'NONE', #12207 ) ;
#4183 = DIRECTION ( 'NONE',  ( 0.5000000000000049960, -0.8660254037844358210, 0.000000000000000000 ) ) ;
#4184 = DIRECTION ( 'NONE',  ( -0.8660254037844370423, -0.5000000000000026645, 0.000000000000000000 ) ) ;
#4185 = FACE_OUTER_BOUND ( 'NONE', #10949, .T. ) ;
#4186 = FACE_OUTER_BOUND ( 'NONE', #9592, .T. ) ;
#4187 = EDGE_CURVE ( 'NONE', #15382, #11167, #15198, .T. ) ;
#4188 = LINE ( 'NONE', #20716, #2442 ) ;
#4189 = CIRCLE ( 'NONE', #17743, 11.94520687646042667 ) ;
#4190 = AXIS2_PLACEMENT_3D ( 'NONE', #1614, #13165, #4892 ) ;
#4191 = ORIENTED_EDGE ( 'NONE', *, *, #6008, .F. ) ;
#4192 = CARTESIAN_POINT ( 'NONE',  ( 30.10683012259193703, -10.00000000000000000, -4.999999999999997335 ) ) ;
#4193 = CARTESIAN_POINT ( 'NONE',  ( 199.2144802262915846, 21.04890371929339921, -14.00000000000005507 ) ) ;
#4194 = CARTESIAN_POINT ( 'NONE',  ( 5.000000000000000000, 7.027796151710712813, -4.057500000000007212 ) ) ;
#4195 = ADVANCED_FACE ( 'NONE', ( #2350 ), #11504, .F. ) ;
#4196 = DIRECTION ( 'NONE',  ( -0.000000000000000000, -0.000000000000000000, 1.000000000000000000 ) ) ;
#4197 = DIRECTION ( 'NONE',  ( -0.8660254037844380415, -0.5000000000000014433, -0.000000000000000000 ) ) ;
#4198 = ADVANCED_FACE ( 'NONE', ( #5801, #12295 ), #7500, .T. ) ;
#4199 = ORIENTED_EDGE ( 'NONE', *, *, #18610, .T. ) ;
#4200 = EDGE_LOOP ( 'NONE', ( #12514, #4332, #15081, #14287 ) ) ;
#4201 = FACE_OUTER_BOUND ( 'NONE', #3006, .T. ) ;
#4202 = VERTEX_POINT ( 'NONE', #4225 ) ;
#4203 = CARTESIAN_POINT ( 'NONE',  ( 210.3388300726135753, 6.082691074106562290, -26.28791492288521425 ) ) ;
#4204 = DIRECTION ( 'NONE',  ( 0.000000000000000000, 0.000000000000000000, 1.000000000000000000 ) ) ;
#4205 = CARTESIAN_POINT ( 'NONE',  ( 184.9952905943349606, 3.535126980567713240, 0.9999999999999876765 ) ) ;
#4206 = AXIS2_PLACEMENT_3D ( 'NONE', #2655, #8795, #1275 ) ;
#4207 =( BOUNDED_CURVE ( )  B_SPLINE_CURVE ( 3, ( #16447, #11575, #14992, #18045 ),
 .UNSPECIFIED., .F., .F. ) 
 B_SPLINE_CURVE_WITH_KNOTS ( ( 4, 4 ),
 ( 4.525516806536070469, 4.712388980384689674 ),
 .UNSPECIFIED. ) 
 CURVE ( )  GEOMETRIC_REPRESENTATION_ITEM ( )  RATIONAL_B_SPLINE_CURVE ( ( 1.000000000000000000, 0.9970920157757060531, 0.9970920157757060531, 1.000000000000000000 ) ) 
 REPRESENTATION_ITEM ( '' )  );
#4208 = EDGE_CURVE ( 'NONE', #11395, #16570, #14097, .T. ) ;
#4209 = DIRECTION ( 'NONE',  ( 0.5000000000000007772, -0.8660254037844381525, 0.000000000000000000 ) ) ;
#4210 = CARTESIAN_POINT ( 'NONE',  ( -20.27070155495306025, 66.46434188593948988, -2.601344003386939718 ) ) ;
#4211 = ORIENTED_EDGE ( 'NONE', *, *, #20410, .F. ) ;
#4212 = ORIENTED_EDGE ( 'NONE', *, *, #10396, .T. ) ;
#4213 = CARTESIAN_POINT ( 'NONE',  ( 26.99999999999999645, 65.00000000000000000, -22.50000000000000000 ) ) ;
#4214 = ADVANCED_FACE ( 'NONE', ( #20635 ), #20435, .T. ) ;
#4215 = CARTESIAN_POINT ( 'NONE',  ( 85.37797649651368204, 230.0773763115391262, -26.99999999999999289 ) ) ;
#4216 = CARTESIAN_POINT ( 'NONE',  ( -21.00073344079603999, 49.53628891258126998, -11.48274257968635759 ) ) ;
#4217 = CARTESIAN_POINT ( 'NONE',  ( -33.99999999999997868, 65.00000000000000000, -12.50000000000000000 ) ) ;
#4218 = AXIS2_PLACEMENT_3D ( 'NONE', #45, #146, #17539 ) ;
#4219 = EDGE_CURVE ( 'NONE', #5521, #7807, #15620, .T. ) ;
#4220 = LINE ( 'NONE', #5477, #17086 ) ;
#4221 = DIRECTION ( 'NONE',  ( -0.8660254037844375974, -0.5000000000000018874, 0.000000000000000000 ) ) ;
#4223 = ORIENTED_EDGE ( 'NONE', *, *, #1409, .F. ) ;
#4222 = VERTEX_POINT ( 'NONE', #1258 ) ;
#4224 = DIRECTION ( 'NONE',  ( 0.8660254037844380415, 0.5000000000000014433, 0.000000000000000000 ) ) ;
#4225 = CARTESIAN_POINT ( 'NONE',  ( -11.09026189855725164, 15.09941697557061957, 0.9457651797582804498 ) ) ;
#4226 = CARTESIAN_POINT ( 'NONE',  ( 1.484819526751606000, 76.25000000000000000, -2.578432583507790810 ) ) ;
#4227 = VERTEX_POINT ( 'NONE', #7385 ) ;
#4228 = VERTEX_POINT ( 'NONE', #18854 ) ;
#4229 = VERTEX_POINT ( 'NONE', #2951 ) ;
#4230 = CARTESIAN_POINT ( 'NONE',  ( 214.1487250227890797, 14.93252232492107545, -20.52105855319947025 ) ) ;
#4231 = CARTESIAN_POINT ( 'NONE',  ( 229.9055306506723753, 36.50734259565051332, -15.69686519029808736 ) ) ;
#4232 = CARTESIAN_POINT ( 'NONE',  ( 1.204199731550535946, 51.70050625791687082, -5.552164477314467383 ) ) ;
#4233 = PLANE ( 'NONE',  #18156 ) ;
#4234 = ORIENTED_EDGE ( 'NONE', *, *, #744, .T. ) ;
#4235 = EDGE_CURVE ( 'NONE', #835, #5696, #15155, .T. ) ;
#4236 = EDGE_CURVE ( 'NONE', #18726, #2385, #18954, .T. ) ;
#4237 = ORIENTED_EDGE ( 'NONE', *, *, #3032, .T. ) ;
#4238 = VERTEX_POINT ( 'NONE', #11105 ) ;
#4239 = CARTESIAN_POINT ( 'NONE',  ( 32.00490953756718682, 238.5222400402097094, -8.999999999999971578 ) ) ;
#4240 = DIRECTION ( 'NONE',  ( -0.8660254037844360431, -0.5000000000000044409, 5.976026924694052093E-17 ) ) ;
#4241 = CARTESIAN_POINT ( 'NONE',  ( 220.5718355850134174, 34.18728306015038498, -10.64970491435236788 ) ) ;
#4242 = AXIS2_PLACEMENT_3D ( 'NONE', #18613, #4089, #16916 ) ;
#4243 = CARTESIAN_POINT ( 'NONE',  ( 214.7133389289038803, 15.25850231560466597, -7.412933984336929960 ) ) ;
#4244 = EDGE_CURVE ( 'NONE', #16739, #18930, #6767, .T. ) ;
#4245 = DIRECTION ( 'NONE',  ( -0.000000000000000000, -0.000000000000000000, 1.000000000000000000 ) ) ;
#4246 = PLANE ( 'NONE',  #9657 ) ;
#4247 = LINE ( 'NONE', #17080, #8890 ) ;
#4248 = CARTESIAN_POINT ( 'NONE',  ( -28.62307079896444506, 76.35052269458219598, -2.692414605357470681 ) ) ;
#4249 = DIRECTION ( 'NONE',  ( -0.5000000000000049960, 0.8660254037844358210, -0.000000000000000000 ) ) ;
#4250 = DIRECTION ( 'NONE',  ( 0.5000000000000044409, -0.8660254037844361541, 0.000000000000000000 ) ) ;
#4251 = VERTEX_POINT ( 'NONE', #7810 ) ;
#4252 = ADVANCED_FACE ( 'NONE', ( #10893 ), #7707, .F. ) ;
#4253 = CARTESIAN_POINT ( 'NONE',  ( 76.09784680959502623, 71.72003589649941091, -0.03901844198412815490 ) ) ;
#4254 = ORIENTED_EDGE ( 'NONE', *, *, #13413, .T. ) ;
#4255 = VECTOR ( 'NONE', #20361, 1000.000000000000114 ) ;
#4256 = ORIENTED_EDGE ( 'NONE', *, *, #13365, .F. ) ;
#4257 = DIRECTION ( 'NONE',  ( 0.000000000000000000, 0.5000000000000014433, 0.8660254037844379305 ) ) ;
#4258 = AXIS2_PLACEMENT_3D ( 'NONE', #8799, #8370, #13690 ) ;
#4259 = CARTESIAN_POINT ( 'NONE',  ( 79.61537190921880836, 55.27319793895139100, -3.834855963081625241 ) ) ;
#4260 = DIRECTION ( 'NONE',  ( 5.600302932053049280E-17, 2.252044633295279187E-17, 1.000000000000000000 ) ) ;
#4261 = CARTESIAN_POINT ( 'NONE',  ( 10.40000000000000568, -3.747002708109903570E-17, -5.400000000000040323 ) ) ;
#4262 = EDGE_LOOP ( 'NONE', ( #5568, #15501, #6738, #5039, #7228, #16402 ) ) ;
#4263 = DIRECTION ( 'NONE',  ( -0.8660254037844362651, -0.5000000000000042188, 6.872020471724002955E-17 ) ) ;
#4264 = VECTOR ( 'NONE', #8528, 999.9999999999998863 ) ;
#4265 = CARTESIAN_POINT ( 'NONE',  ( 196.7914626300884322, 9.035300127502988943, -22.62267072728657169 ) ) ;
#4266 = CARTESIAN_POINT ( 'NONE',  ( -15.99999999999999289, 80.00000000000000000, -12.50000000000000000 ) ) ;
#4267 = CARTESIAN_POINT ( 'NONE',  ( 199.2144802262915846, 21.04890371929339921, -14.00000000000005507 ) ) ;
#4268 = AXIS2_PLACEMENT_3D ( 'NONE', #20053, #16981, #5513 ) ;
#4269 = FACE_OUTER_BOUND ( 'NONE', #19539, .T. ) ;
#4270 = AXIS2_PLACEMENT_3D ( 'NONE', #19694, #11655, #19585 ) ;
#4271 = CARTESIAN_POINT ( 'NONE',  ( 218.3428005204684723, 38.66593341313920007, -12.92165662794185010 ) ) ;
#4272 = CARTESIAN_POINT ( 'NONE',  ( 217.6467332093937159, 37.74020260364051182, -12.62147488791601901 ) ) ;
#4273 = CARTESIAN_POINT ( 'NONE',  ( 9.999999999999994671, 0.000000000000000000, 0.000000000000000000 ) ) ;
#4274 = ORIENTED_EDGE ( 'NONE', *, *, #18627, .F. ) ;
#4275 = DIRECTION ( 'NONE',  ( -0.8660254037844357100, -0.5000000000000051070, 0.000000000000000000 ) ) ;
#4276 = LINE ( 'NONE', #7548, #15935 ) ;
#4277 = B_SPLINE_CURVE_WITH_KNOTS ( 'NONE', 3,
 ( #1228, #15762, #15970, #9467 ),
 .UNSPECIFIED., .F., .F.,
 ( 4, 4 ),
 ( 1.412303226746373230E-05, 0.0006867738243255644111 ),
 .UNSPECIFIED. ) ;
#4278 = AXIS2_PLACEMENT_3D ( 'NONE', #15100, #7115, #13604 ) ;
#4279 = DIRECTION ( 'NONE',  ( 0.000000000000000000, 0.000000000000000000, -1.000000000000000000 ) ) ;
#4280 = CARTESIAN_POINT ( 'NONE',  ( 4.000000000000000000, -3.518949890710766581, 4.553649124439118623E-15 ) ) ;
#4282 = EDGE_LOOP ( 'NONE', ( #144, #17540 ) ) ;
#4281 = VERTEX_POINT ( 'NONE', #6004 ) ;
#4283 = AXIS2_PLACEMENT_3D ( 'NONE', #9401, #17586, #19073 ) ;
#4284 = CARTESIAN_POINT ( 'NONE',  ( 0.3999999999999975797, 7.960204194457795477E-16, -6.500000000000000000 ) ) ;
#4285 = LINE ( 'NONE', #10736, #743 ) ;
#4286 = VECTOR ( 'NONE', #18474, 1000.000000000000114 ) ;
#4287 = ORIENTED_EDGE ( 'NONE', *, *, #7849, .T. ) ;
#4288 = PRODUCT_DEFINITION_CONTEXT ( 'detailed design', #3237, 'design' ) ;
#4289 = CARTESIAN_POINT ( 'NONE',  ( 229.2052127624425850, 36.74086286845060556, -16.00491213559321579 ) ) ;
#4290 = CARTESIAN_POINT ( 'NONE',  ( -35.00000000000000000, 64.25000000000000000, 2.481238266578627449 ) ) ;
#4291 =( LENGTH_UNIT ( ) NAMED_UNIT ( * ) SI_UNIT ( .MILLI., .METRE. ) );
#4292 = DIRECTION ( 'NONE',  ( -0.4999999999999995004, 0.8660254037844390407, 0.000000000000000000 ) ) ;
#4293 = ORIENTED_EDGE ( 'NONE', *, *, #4317, .T. ) ;
#4294 = EDGE_CURVE ( 'NONE', #3810, #16846, #9187, .T. ) ;
#4295 = DIRECTION ( 'NONE',  ( -0.8660254037844355990, -0.5000000000000054401, 1.237624392856779246E-14 ) ) ;
#4296 = ORIENTED_EDGE ( 'NONE', *, *, #10953, .T. ) ;
#4297 = AXIS2_PLACEMENT_3D ( 'NONE', #5280, #3384, #17926 ) ;
#4298 = CARTESIAN_POINT ( 'NONE',  ( 28.00000000000001066, 65.75000000000001421, -1.525597966175989972 ) ) ;
#4299 = CARTESIAN_POINT ( 'NONE',  ( 191.5936596622673278, 35.49346171468947375, -18.97089895516968028 ) ) ;
#4300 = DIRECTION ( 'NONE',  ( -0.000000000000000000, 1.000000000000000000, -0.000000000000000000 ) ) ;
#4301 = B_SPLINE_CURVE_WITH_KNOTS ( 'NONE', 3,
 ( #18161, #10185, #16677, #2158 ),
 .UNSPECIFIED., .F., .F.,
 ( 4, 4 ),
 ( 4.751027867384753061E-07, 0.0004525283445666021943 ),
 .UNSPECIFIED. ) ;
#4302 = LINE ( 'NONE', #10433, #1581 ) ;
#4303 = ORIENTED_EDGE ( 'NONE', *, *, #7230, .F. ) ;
#4304 = ORIENTED_EDGE ( 'NONE', *, *, #18171, .T. ) ;
#4305 = DIRECTION ( 'NONE',  ( -0.5000000000000045519, 0.8660254037844361541, 0.000000000000000000 ) ) ;
#4306 = ORIENTED_EDGE ( 'NONE', *, *, #8567, .F. ) ;
#4307 = ORIENTED_EDGE ( 'NONE', *, *, #8901, .F. ) ;
#4308 = ORIENTED_EDGE ( 'NONE', *, *, #13828, .T. ) ;
#4309 = DIRECTION ( 'NONE',  ( 0.5000000000000051070, -0.8660254037844359321, 0.000000000000000000 ) ) ;
#4310 = CARTESIAN_POINT ( 'NONE',  ( 207.7157532681331134, 10.68739508888871548, -1.717498466822861225 ) ) ;
#4311 = DIRECTION ( 'NONE',  ( -1.000000000000000000, 0.000000000000000000, 0.000000000000000000 ) ) ;
#4312 = DIRECTION ( 'NONE',  ( -0.8660254037844378194, -0.5000000000000013323, -0.000000000000000000 ) ) ;
#4313 = AXIS2_PLACEMENT_3D ( 'NONE', #12928, #14843, #3267 ) ;
#4314 = EDGE_CURVE ( 'NONE', #13886, #20210, #6214, .T. ) ;
#4315 = VERTEX_POINT ( 'NONE', #15483 ) ;
#4316 = AXIS2_PLACEMENT_3D ( 'NONE', #14588, #9575, #9677 ) ;
#4317 = EDGE_CURVE ( 'NONE', #2250, #14420, #12495, .T. ) ;
#4318 = B_SPLINE_CURVE_WITH_KNOTS ( 'NONE', 3,
 ( #20846, #12610, #9508, #6321 ),
 .UNSPECIFIED., .F., .F.,
 ( 4, 4 ),
 ( 4.713673267783319110E-06, 0.0006773644653211034414 ),
 .UNSPECIFIED. ) ;
#4319 = FACE_OUTER_BOUND ( 'NONE', #3948, .T. ) ;
#4320 = CARTESIAN_POINT ( 'NONE',  ( -19.82813546932964144, 50.39885407664990424, -15.93728606778036649 ) ) ;
#4321 = CARTESIAN_POINT ( 'NONE',  ( 195.6791760372415183, 3.738073984511642855, -9.718744748712971671 ) ) ;
#4322 = LINE ( 'NONE', #7598, #12540 ) ;
#4323 = CARTESIAN_POINT ( 'NONE',  ( 191.0833833835251880, 36.99024094849657018, -18.91295074164679235 ) ) ;
#4324 = EDGE_CURVE ( 'NONE', #18930, #5590, #10781, .T. ) ;
#4325 = CIRCLE ( 'NONE', #10049, 4.171999999999999709 ) ;
#4327 = ORIENTED_EDGE ( 'NONE', *, *, #12667, .T. ) ;
#4326 = ORIENTED_EDGE ( 'NONE', *, *, #13282, .T. ) ;
#4328 = CARTESIAN_POINT ( 'NONE',  ( -7.400583024429460366, 65.00000000000000000, -12.50000000000000000 ) ) ;
#4329 =( REPRESENTATION_RELATIONSHIP ('NONE','NONE', #4634, #9638 ) REPRESENTATION_RELATIONSHIP_WITH_TRANSFORMATION ( #217 )SHAPE_REPRESENTATION_RELATIONSHIP( ) );
#4330 = CARTESIAN_POINT ( 'NONE',  ( 206.6184255029011183, 25.32357351780921917, -4.915515517929356371 ) ) ;
#4331 = AXIS2_PLACEMENT_3D ( 'NONE', #18797, #670, #19952 ) ;
#4332 = ORIENTED_EDGE ( 'NONE', *, *, #11381, .T. ) ;
#4333 = ORIENTED_EDGE ( 'NONE', *, *, #10092, .F. ) ;
#4334 = DIRECTION ( 'NONE',  ( 0.000000000000000000, 0.000000000000000000, 1.000000000000000000 ) ) ;
#4335 = DIRECTION ( 'NONE',  ( 0.1997192025788214753, 0.1153079353712215399, 0.9730448705798235842 ) ) ;
#4336 = CARTESIAN_POINT ( 'NONE',  ( 0.6561171340770418636, 58.25694778279074626, 0.9210584346784731480 ) ) ;
#4337 = CARTESIAN_POINT ( 'NONE',  ( -27.23510498666222546, 9.696991385916662765, -5.489464333053563294 ) ) ;
#4338 = ORIENTED_EDGE ( 'NONE', *, *, #16930, .F. ) ;
#4339 = EDGE_CURVE ( 'NONE', #17195, #2385, #1159, .T. ) ;
#4340 = EDGE_LOOP ( 'NONE', ( #11227, #4467, #18364, #14808, #8937, #2021, #8246, #17322, #3805 ) ) ;
#4341 = CARTESIAN_POINT ( 'NONE',  ( 0.8023629684295970899, 72.40585966223045489, 0.5537423545354359655 ) ) ;
#4342 = EDGE_CURVE ( 'NONE', #18395, #12920, #19319, .T. ) ;
#4343 = DIRECTION ( 'NONE',  ( 0.5000000000000052180, -0.8660254037844355990, 2.220446049250312588E-16 ) ) ;
#4344 = CYLINDRICAL_SURFACE ( 'NONE', #15064, 8.000000000000000000 ) ;
#4345 = PRESENTATION_LAYER_ASSIGNMENT (  '', '', ( #11120 ) ) ;
#4346 = PRODUCT_DEFINITION_SHAPE ( 'NONE', 'NONE',  #20957 ) ;
#4347 = DIRECTION ( 'NONE',  ( 0.8660254037844370423, 0.5000000000000026645, -0.000000000000000000 ) ) ;
#4348 = CARTESIAN_POINT ( 'NONE',  ( 199.2144802262915846, 21.04890371929339921, -14.00000000000005507 ) ) ;
#4349 = PLANE ( 'NONE',  #10732 ) ;
#4350 = DIRECTION ( 'NONE',  ( 0.8660254037844370423, 0.5000000000000026645, -0.000000000000000000 ) ) ;
#4351 = DIRECTION ( 'NONE',  ( 0.5000000000000051070, -0.8660254037844358210, 0.000000000000000000 ) ) ;
#4352 = CARTESIAN_POINT ( 'NONE',  ( 5.000000000000004441, -4.685197434473809430, 6.071532165918824830E-15 ) ) ;
#4353 = CARTESIAN_POINT ( 'NONE',  ( 219.8858643771923198, 10.82185380917437278, -17.08769543353844256 ) ) ;
#4354 = ADVANCED_FACE ( 'NONE', ( #15790 ), #14206, .F. ) ;
#4355 = VERTEX_POINT ( 'NONE', #4738 ) ;
#4356 = CARTESIAN_POINT ( 'NONE',  ( 81.76460255947399958, 66.07321026818675591, 0.6318735725429163175 ) ) ;
#4357 = ORIENTED_EDGE ( 'NONE', *, *, #18529, .T. ) ;
#4358 = VECTOR ( 'NONE', #9120, 1000.000000000000227 ) ;
#4359 = VERTEX_POINT ( 'NONE', #3155 ) ;
#4360 = CARTESIAN_POINT ( 'NONE',  ( -3.055511853597258742, 64.25000000000000000, 3.385962996190660768 ) ) ;
#4361 = CARTESIAN_POINT ( 'NONE',  ( 197.6384891630574430, 5.400333206920676865, -21.69368824361338355 ) ) ;
#4362 = EDGE_CURVE ( 'NONE', #1433, #18162, #14606, .T. ) ;
#4363 = APPLICATION_PROTOCOL_DEFINITION ( 'draft international standard', 'automotive_design', 1998, #123 ) ;
#4364 = CARTESIAN_POINT ( 'NONE',  ( 34.99529059433364608, 263.3427481158985302, -28.99999999999997513 ) ) ;
#4365 = ORIENTED_EDGE ( 'NONE', *, *, #17308, .F. ) ;
#4366 = LINE ( 'NONE', #18896, #619 ) ;
#4367 = EDGE_CURVE ( 'NONE', #11709, #17948, #17634, .T. ) ;
#4368 = DIRECTION ( 'NONE',  ( -0.2961981327260292396, -0.1710100716628399076, -0.9396926207859056523 ) ) ;
#4369 = DIRECTION ( 'NONE',  ( 0.000000000000000000, -0.000000000000000000, -1.000000000000000000 ) ) ;
#4370 = DIRECTION ( 'NONE',  ( 0.000000000000000000, -1.117161918529055683E-15, -1.000000000000000000 ) ) ;
#4371 = VECTOR ( 'NONE', #13686, 1000.000000000000114 ) ;
#4372 = DIRECTION ( 'NONE',  ( -0.5000000000000027756, 0.8660254037844372643, -0.000000000000000000 ) ) ;
#4373 = EDGE_CURVE ( 'NONE', #14385, #4177, #2481, .T. ) ;
#4374 = CARTESIAN_POINT ( 'NONE',  ( 219.1556129512320013, 10.40024295182009517, -13.98474561060134747 ) ) ;
#4375 = DIRECTION ( 'NONE',  ( 0.5000000000000052180, -0.8660254037844355990, 1.665334536937734564E-16 ) ) ;
#4376 = EDGE_CURVE ( 'NONE', #16685, #5880, #6436, .T. ) ;
#4377 = LINE ( 'NONE', #4487, #613 ) ;
#4378 = ORIENTED_EDGE ( 'NONE', *, *, #16152, .T. ) ;
#4379 = LINE ( 'NONE', #7757, #14917 ) ;
#4380 = LINE ( 'NONE', #18697, #12901 ) ;
#4381 = EDGE_CURVE ( 'NONE', #16338, #12547, #16101, .T. ) ;
#4382 = ADVANCED_FACE ( 'NONE', ( #6416 ), #14411, .F. ) ;
#4383 = CARTESIAN_POINT ( 'NONE',  ( 159.9952905943347901, 46.83639716978955647, -22.00000000000007816 ) ) ;
#4384 = CARTESIAN_POINT ( 'NONE',  ( -33.46953329182479564, 76.75544209468823453, -3.174647668799659872 ) ) ;
#4385 = ADVANCED_FACE ( 'NONE', ( #90 ), #6729, .T. ) ;
#4387 = ORIENTED_EDGE ( 'NONE', *, *, #7070, .F. ) ;
#4386 = ORIENTED_EDGE ( 'NONE', *, *, #8580, .T. ) ;
#4388 = DIRECTION ( 'NONE',  ( 1.561274065702232331E-18, -4.616915249250367527E-16, 1.000000000000000000 ) ) ;
#4389 = DIRECTION ( 'NONE',  ( 0.000000000000000000, 0.000000000000000000, -1.000000000000000000 ) ) ;
#4390 = EDGE_LOOP ( 'NONE', ( #7986, #1781, #9138, #1628 ) ) ;
#4391 = CARTESIAN_POINT ( 'NONE',  ( 219.5770999726424861, 36.52806405021930658, -17.68583624946726474 ) ) ;
#4392 = FACE_OUTER_BOUND ( 'NONE', #14703, .T. ) ;
#4393 = CARTESIAN_POINT ( 'NONE',  ( 221.4022013937810414, 31.23554090207322176, -13.42327856638907768 ) ) ;
#4394 = VECTOR ( 'NONE', #19723, 1000.000000000000000 ) ;
#4395 = VERTEX_POINT ( 'NONE', #5149 ) ;
#4396 = CARTESIAN_POINT ( 'NONE',  ( 208.4761278624580711, 5.007259451653140125, -14.00000000000005507 ) ) ;
#4397 = EDGE_LOOP ( 'NONE', ( #12714, #15387, #15546, #15107, #13210, #19022 ) ) ;
#4398 = CARTESIAN_POINT ( 'NONE',  ( 198.0735972701637024, -1.389238810292188875, -14.00000000000005507 ) ) ;
#4399 = CARTESIAN_POINT ( 'NONE',  ( 195.2174643819972744, 4.002553897860817500, -13.98704593443225797 ) ) ;
#4400 = CARTESIAN_POINT ( 'NONE',  ( 174.9952905943348469, 20.85563505625644609, -9.000000000000007105 ) ) ;
#4401 = DIRECTION ( 'NONE',  ( 0.000000000000000000, -0.8174753238307713721, -0.5759636229205586933 ) ) ;
#4402 = CIRCLE ( 'NONE', #6404, 5.000000000000039968 ) ;
#4404 = ORIENTED_EDGE ( 'NONE', *, *, #5363, .F. ) ;
#4403 = EDGE_LOOP ( 'NONE', ( #41, #10246, #2498, #3014, #12921 ) ) ;
#4405 = ORIENTED_EDGE ( 'NONE', *, *, #4132, .F. ) ;
#4406 = CARTESIAN_POINT ( 'NONE',  ( 229.0056296929136295, 38.06601677626851910, -11.10922658182128586 ) ) ;
#4407 = ORIENTED_EDGE ( 'NONE', *, *, #8738, .F. ) ;
#4408 = EDGE_LOOP ( 'NONE', ( #15426, #14543, #7872, #11973 ) ) ;
#4409 = EDGE_CURVE ( 'NONE', #1689, #20898, #2058, .T. ) ;
#4410 = DIRECTION ( 'NONE',  ( -0.5000000000000054401, 0.8660254037844354880, -0.000000000000000000 ) ) ;
#4411 = CARTESIAN_POINT ( 'NONE',  ( 20.40444853840588380, 258.6148278819781012, 4.841106397986906451 ) ) ;
#4412 = CARTESIAN_POINT ( 'NONE',  ( 205.0662616026534693, 10.91332106064940888, -14.00000000000005507 ) ) ;
#4413 = LINE ( 'NONE', #923, #5588 ) ;
#4414 = SURFACE_STYLE_USAGE ( .BOTH. , #12587 ) ;
#4415 = AXIS2_PLACEMENT_3D ( 'NONE', #2693, #17105, #7128 ) ;
#4416 = EDGE_LOOP ( 'NONE', ( #11900, #19768, #3772, #5073, #2961 ) ) ;
#4417 = AXIS2_PLACEMENT_3D ( 'NONE', #10195, #16577, #3956 ) ;
#4418 = DIRECTION ( 'NONE',  ( 1.000000000000000000, -0.000000000000000000, -0.000000000000000000 ) ) ;
#4419 = AXIS2_PLACEMENT_3D ( 'NONE', #19297, #17506, #10812 ) ;
#4420 = EDGE_CURVE ( 'NONE', #5696, #13143, #13225, .T. ) ;
#4421 = CARTESIAN_POINT ( 'NONE',  ( 213.9443517339557843, 7.649119109015196649, -24.50020013040646560 ) ) ;
#4422 = CARTESIAN_POINT ( 'NONE',  ( -19.99008258158868756, 49.51761908642668431, -11.85432026588631338 ) ) ;
#4423 = DIRECTION ( 'NONE',  ( -0.8660254037844369313, -0.5000000000000027756, 0.000000000000000000 ) ) ;
#4424 = CYLINDRICAL_SURFACE ( 'NONE', #5728, 9.999999999999994671 ) ;
#4425 = CARTESIAN_POINT ( 'NONE',  ( -28.44688792319594128, 50.84930382153548578, 1.171743096592904765 ) ) ;
#4427 = ORIENTED_EDGE ( 'NONE', *, *, #2952, .F. ) ;
#4426 = ORIENTED_EDGE ( 'NONE', *, *, #1906, .T. ) ;
#4428 = ORIENTED_EDGE ( 'NONE', *, *, #61, .F. ) ;
#4429 = CIRCLE ( 'NONE', #16965, 1.500000000000000444 ) ;
#4430 = FACE_OUTER_BOUND ( 'NONE', #14929, .T. ) ;
#4431 = DIRECTION ( 'NONE',  ( -0.5000000000000049960, 0.8660254037844357100, -0.000000000000000000 ) ) ;
#4432 = EDGE_CURVE ( 'NONE', #6530, #7581, #20327, .T. ) ;
#4433 = VECTOR ( 'NONE', #14568, 1000.000000000000114 ) ;
#4434 = ORIENTED_EDGE ( 'NONE', *, *, #14083, .F. ) ;
#4435 = ORIENTED_EDGE ( 'NONE', *, *, #19079, .F. ) ;
#4436 = ORIENTED_EDGE ( 'NONE', *, *, #4972, .F. ) ;
#4437 = EDGE_CURVE ( 'NONE', #2398, #1492, #8827, .T. ) ;
#4438 = CARTESIAN_POINT ( 'NONE',  ( 207.3877668936371492, 11.02908132907535332, -2.195132782454303655 ) ) ;
#4439 = DIRECTION ( 'NONE',  ( -5.175391130484829193E-17, -2.988013462347053780E-17, -1.000000000000000000 ) ) ;
#4440 = CARTESIAN_POINT ( 'NONE',  ( -3.198494086879704934, 50.00375224366489846, -12.08029061943339322 ) ) ;
#4441 = CARTESIAN_POINT ( 'NONE',  ( -25.99999999999999645, 9.999999999999994671, 7.500000000000000000 ) ) ;
#4442 = EDGE_LOOP ( 'NONE', ( #20192, #20407, #4526, #18482, #344, #15073 ) ) ;
#4443 = AXIS2_PLACEMENT_3D ( 'NONE', #13124, #8334, #289 ) ;
#4444 = ADVANCED_FACE ( 'NONE', ( #285 ), #6522, .T. ) ;
#4445 = ORIENTED_EDGE ( 'NONE', *, *, #2652, .F. ) ;
#4446 = CARTESIAN_POINT ( 'NONE',  ( 1.317725315667332309, 74.84505238333373711, -1.139833306050669126 ) ) ;
#4447 = ORIENTED_EDGE ( 'NONE', *, *, #7821, .T. ) ;
#4448 = AXIS2_PLACEMENT_3D ( 'NONE', #20388, #18915, #4389 ) ;
#4449 = FACE_OUTER_BOUND ( 'NONE', #5559, .T. ) ;
#4450 = VECTOR ( 'NONE', #12967, 1000.000000000000227 ) ;
#4451 = DIRECTION ( 'NONE',  ( 0.000000000000000000, 0.000000000000000000, -1.000000000000000000 ) ) ;
#4452 = CARTESIAN_POINT ( 'NONE',  ( 80.48184134440170112, 67.67503062758028420, -25.55523453281406887 ) ) ;
#4453 = VECTOR ( 'NONE', #20412, 1000.000000000000227 ) ;
#4454 = VECTOR ( 'NONE', #3132, 1000.000000000000000 ) ;
#4455 = DIRECTION ( 'NONE',  ( 0.000000000000000000, 0.000000000000000000, -1.000000000000000000 ) ) ;
#4456 = CARTESIAN_POINT ( 'NONE',  ( 211.6640881527417832, 17.62201447656351405, -23.53124788243930965 ) ) ;
#4457 = DIRECTION ( 'NONE',  ( 0.5000000000000051070, -0.8660254037844359321, 0.000000000000000000 ) ) ;
#4458 = APPLICATION_CONTEXT ( 'automotive_design' ) ;
#4459 = EDGE_LOOP ( 'NONE', ( #3387, #15764, #3855, #6224, #4735, #10983, #13645, #762, #170, #20097, #10114, #5739, #5308, #8438, #13970, #3680, #76, #9865, #16053, #7554, #20276, #14749, #2251, #14766, #7822, #1088, #7198, #17032, #294, #11634, #16633, #10079, #18461, #17234, #11372, #16300, #7286, #11964, #13802, #12786, #9975, #17663, #18929, #7085, #7795, #2980, #3265, #14059, #14436, #5440, #1079, #11244 ) ) ;
#4460 = DIRECTION ( 'NONE',  ( 0.000000000000000000, 1.000000000000000000, -1.295896757998782163E-15 ) ) ;
#4461 = DIRECTION ( 'NONE',  ( -0.5000000000000045519, 0.8660254037844360431, 4.006172263299081054E-16 ) ) ;
#4462 = PLANE ( 'NONE',  #18357 ) ;
#4463 = VERTEX_POINT ( 'NONE', #11416 ) ;
#4464 = CARTESIAN_POINT ( 'NONE',  ( 72.13472612272360607, 72.43562250713796402, -1.655863322246043268 ) ) ;
#4465 = ADVANCED_FACE ( 'NONE', ( #19675 ), #13580, .T. ) ;
#4466 = MECHANICAL_DESIGN_GEOMETRIC_PRESENTATION_REPRESENTATION (  '', ( #7839 ), #20373 ) ;
#4467 = ORIENTED_EDGE ( 'NONE', *, *, #16106, .T. ) ;
#4468 = EDGE_CURVE ( 'NONE', #1190, #3202, #9031, .T. ) ;
#4469 = EDGE_LOOP ( 'NONE', ( #8428, #20734, #15410, #16750 ) ) ;
#4470 = CARTESIAN_POINT ( 'NONE',  ( 0.7787292174182174342, 72.29984585682862530, 0.6063817381306070287 ) ) ;
#4471 = VECTOR ( 'NONE', #14316, 1000.000000000000114 ) ;
#4472 = VECTOR ( 'NONE', #17107, 1000.000000000000227 ) ;
#4473 = CARTESIAN_POINT ( 'NONE',  ( 229.7512887155055239, 36.77449746401691044, -13.55260094074461819 ) ) ;
#4474 = ADVANCED_FACE ( 'NONE', ( #9809 ), #8221, .F. ) ;
#4475 = ORIENTED_EDGE ( 'NONE', *, *, #4694, .T. ) ;
#4476 = LINE ( 'NONE', #18685, #13839 ) ;
#4477 = CARTESIAN_POINT ( 'NONE',  ( 226.0241994620535024, 43.23000541533971841, -14.55761806292083982 ) ) ;
#4478 = DIRECTION ( 'NONE',  ( 1.000000000000000000, 0.000000000000000000, 0.000000000000000000 ) ) ;
#4479 = CARTESIAN_POINT ( 'NONE',  ( -11.10102051443364779, 14.09941697557065332, 0.9999999999999991118 ) ) ;
#4480 = VECTOR ( 'NONE', #13848, 1000.000000000000114 ) ;
#4481 = CARTESIAN_POINT ( 'NONE',  ( 226.5540741482489295, 42.31223553720493413, -11.78314368930802303 ) ) ;
#4482 = CARTESIAN_POINT ( 'NONE',  ( 199.2231352798572743, 21.03391272677540513, -14.00000000000005507 ) ) ;
#4483 = EDGE_CURVE ( 'NONE', #8913, #8276, #19370, .T. ) ;
#4484 = AXIS2_PLACEMENT_3D ( 'NONE', #17049, #13662, #18636 ) ;
#4485 = LINE ( 'NONE', #12339, #5183 ) ;
#4486 = FACE_OUTER_BOUND ( 'NONE', #4840, .T. ) ;
#4487 = CARTESIAN_POINT ( 'NONE',  ( 205.5254235590769838, 9.953856903543536916, -15.84972809015757278 ) ) ;
#4488 = ORIENTED_EDGE ( 'NONE', *, *, #1563, .F. ) ;
#4489 = DIRECTION ( 'NONE',  ( -0.03412120668233696585, 0.05909966358936712821, 0.9976687691905389288 ) ) ;
#4490 = ADVANCED_FACE ( 'NONE', ( #16607 ), #3989, .F. ) ;
#4491 = DIRECTION ( 'NONE',  ( 0.4661719196087402706, -0.8846941513134933821, 4.730853538934608585E-18 ) ) ;
#4492 = DIRECTION ( 'NONE',  ( -0.000000000000000000, -0.000000000000000000, 1.000000000000000000 ) ) ;
#4493 = CARTESIAN_POINT ( 'NONE',  ( 211.5944766886066191, 17.58182427900635503, -4.392917125964958203 ) ) ;
#4494 = DIRECTION ( 'NONE',  ( -0.06808332454812729417, 0.1179237772655570560, 0.9906859460363297565 ) ) ;
#4496 = ORIENTED_EDGE ( 'NONE', *, *, #4752, .T. ) ;
#4495 = ORIENTED_EDGE ( 'NONE', *, *, #5131, .F. ) ;
#4497 = CARTESIAN_POINT ( 'NONE',  ( -14.69480916118295255, 10.26995882791192471, 12.43268610818004838 ) ) ;
#4498 = SURFACE_STYLE_USAGE ( .BOTH. , #9564 ) ;
#4499 = UNCERTAINTY_MEASURE_WITH_UNIT (LENGTH_MEASURE( 1.000000000000000082E-05 ), #54, 'distance_accuracy_value', 'NONE');
#4500 = VECTOR ( 'NONE', #12225, 1000.000000000000000 ) ;
#4501 = ADVANCED_FACE ( 'NONE', ( #10439 ), #2075, .F. ) ;
#4502=STYLED_ITEM('',(#20974),#10712);
#4503 = LINE ( 'NONE', #15847, #20517 ) ;
#4504 = EDGE_CURVE ( 'NONE', #9864, #1927, #14954, .T. ) ;
#4505 = DIRECTION ( 'NONE',  ( 0.4999999999999995004, -0.8660254037844390407, 0.000000000000000000 ) ) ;
#4506 = DIRECTION ( 'NONE',  ( 0.5000000000000054401, -0.8660254037844354880, 0.000000000000000000 ) ) ;
#4507 = DIRECTION ( 'NONE',  ( -0.8660254037844354880, -0.5000000000000055511, 0.000000000000000000 ) ) ;
#4508 = EDGE_CURVE ( 'NONE', #1201, #20315, #17654, .T. ) ;
#4509 = ORIENTED_EDGE ( 'NONE', *, *, #11330, .T. ) ;
#4510 = DIRECTION ( 'NONE',  ( 1.000000000000000000, 0.000000000000000000, 0.000000000000000000 ) ) ;
#4511 = CARTESIAN_POINT ( 'NONE',  ( 221.4641624591582172, 32.64172757717244622, -12.10162843130820853 ) ) ;
#4512 = AXIS2_PLACEMENT_3D ( 'NONE', #7275, #2529, #18847 ) ;
#4513 = DIRECTION ( 'NONE',  ( 0.8660254037844352659, 0.5000000000000056621, 0.000000000000000000 ) ) ;
#4514 = CARTESIAN_POINT ( 'NONE',  ( -15.99999999999999289, 9.999999999999994671, 0.000000000000000000 ) ) ;
#4515 = ORIENTED_EDGE ( 'NONE', *, *, #1997, .T. ) ;
#4516 = DIRECTION ( 'NONE',  ( -0.8660254037844357100, -0.5000000000000051070, 0.000000000000000000 ) ) ;
#4517 = ADVANCED_FACE ( 'NONE', ( #10116 ), #3092, .T. ) ;
#4518 = VERTEX_POINT ( 'NONE', #3880 ) ;
#4519 = ORIENTED_EDGE ( 'NONE', *, *, #2033, .F. ) ;
#4520 = DIRECTION ( 'NONE',  ( 0.8660254037844352659, 0.5000000000000056621, 0.000000000000000000 ) ) ;
#4521 = CARTESIAN_POINT ( 'NONE',  ( 219.5483150135131325, 35.03133031408865605, -14.00000000000005507 ) ) ;
#4522 = CARTESIAN_POINT ( 'NONE',  ( 218.9852377222535154, 11.07469685814948157, -16.89203719259520753 ) ) ;
#4523 = DIRECTION ( 'NONE',  ( -0.5000000000000054401, 0.8660254037844354880, -0.000000000000000000 ) ) ;
#4524 = CARTESIAN_POINT ( 'NONE',  ( 226.0051869642230429, 43.26293602756123136, -15.69686519029800387 ) ) ;
#4525 = AXIS2_PLACEMENT_3D ( 'NONE', #14563, #14463, #7862 ) ;
#4526 = ORIENTED_EDGE ( 'NONE', *, *, #16699, .F. ) ;
#4527 = DIRECTION ( 'NONE',  ( 0.4999999999999995004, -0.8660254037844390407, 0.000000000000000000 ) ) ;
#4528 = ORIENTED_EDGE ( 'NONE', *, *, #1881, .F. ) ;
#4529 = CARTESIAN_POINT ( 'NONE',  ( 211.2164883113428857, 12.70854540844746872, -3.188775577416895324 ) ) ;
#4530 = CARTESIAN_POINT ( 'NONE',  ( -4.094320337108634966, 46.27675487045426905, -3.861523532182237428 ) ) ;
#4531 = CARTESIAN_POINT ( 'NONE',  ( 0.000000000000000000, 0.000000000000000000, 0.000000000000000000 ) ) ;
#4532 = CARTESIAN_POINT ( 'NONE',  ( 193.6336827526812101, 7.212155065240265728, -15.39542905462715083 ) ) ;
#4533 = CARTESIAN_POINT ( 'NONE',  ( -24.14678699472350587, 45.01203632813575695, -9.488349599000542867 ) ) ;
#4535 = VERTEX_POINT ( 'NONE', #13333 ) ;
#4534 = EDGE_LOOP ( 'NONE', ( #1316, #5052, #8100, #12206, #17872, #17188 ) ) ;
#4536 = ORIENTED_EDGE ( 'NONE', *, *, #12483, .F. ) ;
#4537 = CIRCLE ( 'NONE', #3500, 13.50000000000000711 ) ;
#4538 = CARTESIAN_POINT ( 'NONE',  ( 227.8114636848558519, 40.13437297489625166, -18.24372585368654498 ) ) ;
#4539 = DIRECTION ( 'NONE',  ( -0.8660254037844361541, -0.5000000000000044409, 5.976026924694052093E-17 ) ) ;
#4540 = ORIENTED_EDGE ( 'NONE', *, *, #2575, .T. ) ;
#4541 = ORIENTED_EDGE ( 'NONE', *, *, #5697, .F. ) ;
#4542 = DIRECTION ( 'NONE',  ( 0.4586056507527294102, -0.7943282877419115540, -0.3984010898462361783 ) ) ;
#4543 = CARTESIAN_POINT ( 'NONE',  ( 228.9008876695278900, 37.92096620649393657, -10.98877789909422020 ) ) ;
#4544 = CARTESIAN_POINT ( 'NONE',  ( -4.472320007499605232, 50.00706524506586703, -13.00541661879220356 ) ) ;
#4545 = CARTESIAN_POINT ( 'NONE',  ( -28.43148821208374244, 8.662657545001765769, 1.350916757379553967 ) ) ;
#4546 = ORIENTED_EDGE ( 'NONE', *, *, #16748, .T. ) ;
#4547 = EDGE_LOOP ( 'NONE', ( #18187, #10048, #18006, #9329, #9920 ) ) ;
#4548 = CARTESIAN_POINT ( 'NONE',  ( 0.02492996559929827605, 68.25592811474754740, 2.150873336511314626 ) ) ;
#4549 = AXIS2_PLACEMENT_3D ( 'NONE', #12070, #20323, #10454 ) ;
#4550 =( NAMED_UNIT ( * ) PLANE_ANGLE_UNIT ( ) SI_UNIT ( $, .RADIAN. ) );
#4551 = LINE ( 'NONE', #11401, #9271 ) ;
#4552 = ORIENTED_EDGE ( 'NONE', *, *, #9413, .T. ) ;
#4553 = VECTOR ( 'NONE', #16703, 1000.000000000000227 ) ;
#4554 = LINE ( 'NONE', #4753, #8418 ) ;
#4555 = CARTESIAN_POINT ( 'NONE',  ( 71.78648230981508505, 75.22576515165123112, -23.93658930654907380 ) ) ;
#4556 = EDGE_CURVE ( 'NONE', #7000, #5435, #8653, .T. ) ;
#4557 = CARTESIAN_POINT ( 'NONE',  ( 195.4194262334934535, 4.119156627188157671, -15.39542905462715083 ) ) ;
#4558 = DIRECTION ( 'NONE',  ( 0.000000000000000000, 0.000000000000000000, 1.000000000000000000 ) ) ;
#4559 = CARTESIAN_POINT ( 'NONE',  ( 220.9043665878753302, 33.58129766204038447, -11.00782313096298104 ) ) ;
#4560 = ORIENTED_EDGE ( 'NONE', *, *, #15377, .T. ) ;
#4561 = DIRECTION ( 'NONE',  ( 0.000000000000000000, 0.000000000000000000, -1.000000000000000000 ) ) ;
#4562 = LINE ( 'NONE', #7932, #20108 ) ;
#4563 = FACE_OUTER_BOUND ( 'NONE', #13048, .T. ) ;
#4564 = VERTEX_POINT ( 'NONE', #8860 ) ;
#4565 = CARTESIAN_POINT ( 'NONE',  ( 78.57212408006208193, 68.17132923325316085, 0.1403190541435616057 ) ) ;
#4566 = ORIENTED_EDGE ( 'NONE', *, *, #14196, .T. ) ;
#4567 = VERTEX_POINT ( 'NONE', #1984 ) ;
#4568 = CARTESIAN_POINT ( 'NONE',  ( -3.979955202765648181, 75.03053098945672161, 3.432994178268343965 ) ) ;
#4569 = AXIS2_PLACEMENT_3D ( 'NONE', #19235, #3013, #19428 ) ;
#4570 = DIRECTION ( 'NONE',  ( 0.000000000000000000, -1.000000000000000000, 0.000000000000000000 ) ) ;
#4571 = EDGE_CURVE ( 'NONE', #6530, #7909, #2965, .T. ) ;
#4572 = CARTESIAN_POINT ( 'NONE',  ( 201.0721825858487364, 0.7325896531374328502, -4.915515517929136990 ) ) ;
#4573 = ORIENTED_EDGE ( 'NONE', *, *, #14693, .F. ) ;
#4574 = APPLICATION_PROTOCOL_DEFINITION ( 'draft international standard', 'automotive_design', 1998, #2972 ) ;
#4575 = CARTESIAN_POINT ( 'NONE',  ( 37.00490953756721524, 229.8619860023653985, 26.00000000000001776 ) ) ;
#4576 = ORIENTED_EDGE ( 'NONE', *, *, #4034, .F. ) ;
#4577 = DIRECTION ( 'NONE',  ( 0.4758887346169485832, 0.2747544890354092773, 0.8354878114129317135 ) ) ;
#4578 = CARTESIAN_POINT ( 'NONE',  ( 215.5602275462317436, 15.57044378260907180, -9.848357292554322129 ) ) ;
#4579 = DIRECTION ( 'NONE',  ( -0.000000000000000000, 1.000000000000000000, -0.000000000000000000 ) ) ;
#4580 = DIRECTION ( 'NONE',  ( 0.000000000000000000, 6.938893903907178303E-18, 1.000000000000000000 ) ) ;
#4581 = EDGE_CURVE ( 'NONE', #18042, #1689, #6725, .T. ) ;
#4582 = EDGE_CURVE ( 'NONE', #4151, #18967, #15361, .T. ) ;
#4583 = CARTESIAN_POINT ( 'NONE',  ( 208.0983737146324870, 5.661548828456886895, -14.00000000000005507 ) ) ;
#4584 = CARTESIAN_POINT ( 'NONE',  ( 217.6183575532813848, 31.03031750895123508, -14.00000000000004441 ) ) ;
#4585 = FACE_OUTER_BOUND ( 'NONE', #15163, .T. ) ;
#4586 = CARTESIAN_POINT ( 'NONE',  ( 201.9688168050318211, 0.4774415703040005288, -3.480441514389559288 ) ) ;
#4587 = CIRCLE ( 'NONE', #17116, 12.47473710546057823 ) ;
#4588 = LINE ( 'NONE', #9442, #1296 ) ;
#4589 = VERTEX_POINT ( 'NONE', #7056 ) ;
#4590 = DIRECTION ( 'NONE',  ( -0.8660254037844363761, -0.5000000000000043299, 6.872020471724002955E-17 ) ) ;
#4591 = FACE_OUTER_BOUND ( 'NONE', #12229, .T. ) ;
#4592 = EDGE_CURVE ( 'NONE', #8802, #3117, #813, .T. ) ;
#4593 = DIRECTION ( 'NONE',  ( -0.5000000000000051070, 0.8660254037844359321, -0.000000000000000000 ) ) ;
#4594 = DIRECTION ( 'NONE',  ( 0.000000000000000000, 0.000000000000000000, -1.000000000000000000 ) ) ;
#4596 = VERTEX_POINT ( 'NONE', #6949 ) ;
#4595 = VERTEX_POINT ( 'NONE', #507 ) ;
#4597 = EDGE_CURVE ( 'NONE', #9257, #7667, #7182, .T. ) ;
#4598 = CARTESIAN_POINT ( 'NONE',  ( 191.5478494775925640, 36.18576207517880050, -14.00000000000006395 ) ) ;
#4599 = VERTEX_POINT ( 'NONE', #8549 ) ;
#4600 = VECTOR ( 'NONE', #17720, 1000.000000000000227 ) ;
#4601 = PLANE ( 'NONE',  #8718 ) ;
#4602 = CARTESIAN_POINT ( 'NONE',  ( 205.0662616026534693, 10.91332106064940888, -14.00000000000005507 ) ) ;
#4603 = ORIENTED_EDGE ( 'NONE', *, *, #5344, .T. ) ;
#4604 = EDGE_CURVE ( 'NONE', #4855, #18774, #12621, .T. ) ;
#4605 = LINE ( 'NONE', #2610, #5814 ) ;
#4606 = ORIENTED_EDGE ( 'NONE', *, *, #19004, .T. ) ;
#4607 = FACE_OUTER_BOUND ( 'NONE', #4083, .T. ) ;
#4608 = LINE ( 'NONE', #1437, #15842 ) ;
#4609 = AXIS2_PLACEMENT_3D ( 'NONE', #15774, #14079, #20313 ) ;
#4610 = ADVANCED_FACE ( 'NONE', ( #16719 ), #2198, .F. ) ;
#4611 = DIRECTION ( 'NONE',  ( -0.000000000000000000, -1.000000000000000000, -0.000000000000000000 ) ) ;
#4612 = DIRECTION ( 'NONE',  ( 1.000000000000000000, 0.000000000000000000, 0.000000000000000000 ) ) ;
#4613 = EDGE_CURVE ( 'NONE', #13544, #16413, #604, .T. ) ;
#4614 = AXIS2_PLACEMENT_3D ( 'NONE', #14941, #8018, #405 ) ;
#4615 = ORIENTED_EDGE ( 'NONE', *, *, #20040, .F. ) ;
#4616 = AXIS2_PLACEMENT_3D ( 'NONE', #1384, #3076, #1801 ) ;
#4617 = CARTESIAN_POINT ( 'NONE',  ( 114.2964607176050578, 65.98909236273156864, -7.887051853916060842E-15 ) ) ;
#4618 = EDGE_LOOP ( 'NONE', ( #20810, #14203 ) ) ;
#4619 = DIRECTION ( 'NONE',  ( -0.5000000000000052180, 0.8660254037844355990, 0.000000000000000000 ) ) ;
#4620 = CARTESIAN_POINT ( 'NONE',  ( 210.8300749258795577, 17.14049671552684728, -22.62267072728681683 ) ) ;
#4621 = DIRECTION ( 'NONE',  ( 0.1005394128318083391, 0.05804645706261228610, -0.9932383577419438003 ) ) ;
#4622 = EDGE_CURVE ( 'NONE', #9607, #13077, #8793, .T. ) ;
#4623 = FACE_OUTER_BOUND ( 'NONE', #13097, .T. ) ;
#4624 = FACE_OUTER_BOUND ( 'NONE', #6834, .T. ) ;
#4625 = EDGE_LOOP ( 'NONE', ( #8035, #2118, #9734, #14828 ) ) ;
#4626 = AXIS2_PLACEMENT_3D ( 'NONE', #17509, #2987, #3090 ) ;
#4627 = DIRECTION ( 'NONE',  ( 0.8660254037844352659, 0.5000000000000056621, 0.000000000000000000 ) ) ;
#4628 = ADVANCED_FACE ( 'NONE', ( #13749 ), #5057, .F. ) ;
#4629 = FACE_OUTER_BOUND ( 'NONE', #14208, .T. ) ;
#4630 = CARTESIAN_POINT ( 'NONE',  ( -7.082764429467357736, 50.04906111657209067, -8.763765402883818112 ) ) ;
#4631 = FACE_OUTER_BOUND ( 'NONE', #15976, .T. ) ;
#4632 = EDGE_CURVE ( 'NONE', #12877, #5200, #7093, .T. ) ;
#4633 = LINE ( 'NONE', #19160, #19626 ) ;
#4634 = SHAPE_REPRESENTATION ( 'MAS-328', ( #3015, #7039, #5008, #19566, #20255, #6694, #18572, #8397, #9412, #11122, #1985, #10082, #974, #12828 ), #10795 ) ;
#4635 = CARTESIAN_POINT ( 'NONE',  ( 5.000000000000000000, 0.000000000000000000, 0.000000000000000000 ) ) ;
#4636 = ADVANCED_FACE ( 'NONE', ( #17422 ), #1354, .T. ) ;
#4638 = ORIENTED_EDGE ( 'NONE', *, *, #376, .F. ) ;
#4637 = ORIENTED_EDGE ( 'NONE', *, *, #5054, .F. ) ;
#4639 = FACE_OUTER_BOUND ( 'NONE', #14377, .T. ) ;
#4640 = CARTESIAN_POINT ( 'NONE',  ( 192.4175317442008009, 6.510009953118869319, -14.05525385477287870 ) ) ;
#4641 = LINE ( 'NONE', #7501, #12476 ) ;
#4642 = ORIENTED_EDGE ( 'NONE', *, *, #2566, .T. ) ;
#4643 = EDGE_LOOP ( 'NONE', ( #16156, #155, #1489, #18989, #4013, #10388 ) ) ;
#4644 = CIRCLE ( 'NONE', #924, 3.902363844300875240 ) ;
#4645 = DIRECTION ( 'NONE',  ( 0.000000000000000000, 0.6846849967427295347, 0.7288391147814505810 ) ) ;
#4646 = AXIS2_PLACEMENT_3D ( 'NONE', #19088, #17498, #2975 ) ;
#4647 = DIRECTION ( 'NONE',  ( -0.000000000000000000, 1.000000000000000000, -0.000000000000000000 ) ) ;
#4648 = CARTESIAN_POINT ( 'NONE',  ( -32.10259343984367320, 61.14548605613433097, 2.017374915500129706 ) ) ;
#4649 = CARTESIAN_POINT ( 'NONE',  ( -28.48674344962430283, 8.589208059839100073, 0.6694126349350221217 ) ) ;
#4650 = ORIENTED_EDGE ( 'NONE', *, *, #2504, .F. ) ;
#4651 = ORIENTED_EDGE ( 'NONE', *, *, #1914, .T. ) ;
#4652 = DIRECTION ( 'NONE',  ( -0.8660254037844344888, -0.5000000000000069944, 0.000000000000000000 ) ) ;
#4653 = CARTESIAN_POINT ( 'NONE',  ( 226.2066167028222594, 42.91404948615199544, -14.93232347545819216 ) ) ;
#4654 = VECTOR ( 'NONE', #11850, 999.9999999999998863 ) ;
#4655 = CYLINDRICAL_SURFACE ( 'NONE', #15996, 3.902363844300889451 ) ;
#4656 = CARTESIAN_POINT ( 'NONE',  ( -27.42628672828266545, 60.97609658108721931, 5.069224955254768794 ) ) ;
#4657 = LINE ( 'NONE', #15909, #14353 ) ;
#4658 = VECTOR ( 'NONE', #20554, 1000.000000000000000 ) ;
#4659 = LINE ( 'NONE', #17601, #10033 ) ;
#4660 = CARTESIAN_POINT ( 'NONE',  ( 98.91428619100422281, 200.0914894846855248, 11.00000000000001066 ) ) ;
#4661 = DIRECTION ( 'NONE',  ( 0.8660254037844370423, 0.5000000000000026645, -0.000000000000000000 ) ) ;
#4662 = ORIENTED_EDGE ( 'NONE', *, *, #11730, .T. ) ;
#4663 = CARTESIAN_POINT ( 'NONE',  ( 81.71790390665692883, 62.87457526787128614, 0.3277555819696695849 ) ) ;
#4664 = ORIENTED_EDGE ( 'NONE', *, *, #19776, .F. ) ;
#4665 = EDGE_LOOP ( 'NONE', ( #17748, #9634, #16786, #4008 ) ) ;
#4666 = CARTESIAN_POINT ( 'NONE',  ( -3.297392717249913119, 67.76582539289996987, 2.255487788202362509 ) ) ;
#4667 = CARTESIAN_POINT ( 'NONE',  ( 208.8577037357181894, 4.346350652224121092, -14.00000000000005507 ) ) ;
#4668 = AXIS2_PLACEMENT_3D ( 'NONE', #5861, #15753, #14055 ) ;
#4669 = ADVANCED_FACE ( 'NONE', ( #4690 ), #18265, .T. ) ;
#4670 = LINE ( 'NONE', #17614, #19520 ) ;
#4671 = SHAPE_DEFINITION_REPRESENTATION ( #15533, #6911 ) ;
#4672 = DIRECTION ( 'NONE',  ( -0.5000000000000043299, 0.8660254037844361541, 1.272130549049658700E-16 ) ) ;
#4673 = EDGE_LOOP ( 'NONE', ( #5151, #12437 ) ) ;
#4674 = SURFACE_SIDE_STYLE ('',( #19303 ) ) ;
#4675 = CARTESIAN_POINT ( 'NONE',  ( 195.3111273346253824, 3.525580966981323616, -11.13829696442576811 ) ) ;
#4676 = DIRECTION ( 'NONE',  ( 0.000000000000000000, 0.000000000000000000, 1.000000000000000000 ) ) ;
#4677 = CARTESIAN_POINT ( 'NONE',  ( 61.99529059433388767, 216.5773763115390693, -28.99999999999998934 ) ) ;
#4678 = EDGE_LOOP ( 'NONE', ( #3147, #20446, #18491, #5135 ) ) ;
#4679 = DIRECTION ( 'NONE',  ( 0.5000000000000046629, -0.8660254037844360431, 0.000000000000000000 ) ) ;
#4680 = DIRECTION ( 'NONE',  ( 0.000000000000000000, 6.938893903907177533E-18, 1.000000000000000000 ) ) ;
#4681 = CARTESIAN_POINT ( 'NONE',  ( 103.4382437392645642, 216.2557651598135919, 11.00000000000001066 ) ) ;
#4682 = EDGE_CURVE ( 'NONE', #4077, #16512, #18946, .T. ) ;
#4683 = CARTESIAN_POINT ( 'NONE',  ( -31.74999999999995737, 0.000000000000000000, 0.000000000000000000 ) ) ;
#4684 = DIRECTION ( 'NONE',  ( -0.4084849465052255435, 0.7075166814741008503, 0.5766803221148599778 ) ) ;
#4685 = VECTOR ( 'NONE', #16040, 1000.000000000000000 ) ;
#4686 = DIRECTION ( 'NONE',  ( 0.8660254037844370423, 0.5000000000000026645, -0.000000000000000000 ) ) ;
#4687 = VERTEX_POINT ( 'NONE', #9663 ) ;
#4688 = CARTESIAN_POINT ( 'NONE',  ( 195.3479444306255175, 4.077886589060220501, -13.97827067520021416 ) ) ;
#4689 = CARTESIAN_POINT ( 'NONE',  ( 82.94492693169769382, 61.96459963853332198, 0.3444023811076172281 ) ) ;
#4690 = FACE_OUTER_BOUND ( 'NONE', #906, .T. ) ;
#4691 = EDGE_CURVE ( 'NONE', #17545, #4687, #14368, .T. ) ;
#4693 = ORIENTED_EDGE ( 'NONE', *, *, #10164, .T. ) ;
#4692 = ORIENTED_EDGE ( 'NONE', *, *, #8214, .T. ) ;
#4694 = EDGE_CURVE ( 'NONE', #16413, #17073, #3005, .T. ) ;
#4695 = SURFACE_SIDE_STYLE ('',( #7766 ) ) ;
#4696 = PLANE ( 'NONE',  #16470 ) ;
#4697 = AXIS2_PLACEMENT_3D ( 'NONE', #2993, #13057, #20782 ) ;
#4698 = ORIENTED_EDGE ( 'NONE', *, *, #10799, .F. ) ;
#4699 = LINE ( 'NONE', #3118, #19885 ) ;
#4700 = CARTESIAN_POINT ( 'NONE',  ( -28.42369844106826093, 79.61691370731600159, -9.098688494702861007 ) ) ;
#4701 = CARTESIAN_POINT ( 'NONE',  ( 62.36389338619030553, 105.9389375482328006, -12.50000000000000000 ) ) ;
#4702 = ORIENTED_EDGE ( 'NONE', *, *, #15115, .T. ) ;
#4703 = VERTEX_POINT ( 'NONE', #15945 ) ;
#4704 = DIRECTION ( 'NONE',  ( 0.5000000000000054401, -0.8660254037844354880, 0.000000000000000000 ) ) ;
#4705 = VERTEX_POINT ( 'NONE', #17633 ) ;
#4706 = CARTESIAN_POINT ( 'NONE',  ( 22.00490953756706958, 255.8427481158984165, 1.000000000000018208 ) ) ;
#4707 = PRODUCT_RELATED_PRODUCT_CATEGORY ( 'part', '', ( #16509 ) ) ;
#4708 = DIRECTION ( 'NONE',  ( 0.000000000000000000, -1.000000000000000000, 1.110768649713242108E-15 ) ) ;
#4709 = ADVANCED_FACE ( 'NONE', ( #19120 ), #20699, .F. ) ;
#4710 = CARTESIAN_POINT ( 'NONE',  ( 4.000000000000000000, -1.759474945355379072, 3.047500000000001652 ) ) ;
#4711 = CARTESIAN_POINT ( 'NONE',  ( 227.1552142281217925, 41.27103037639910355, -10.80501622924628258 ) ) ;
#4712 = VECTOR ( 'NONE', #8797, 1000.000000000000227 ) ;
#4713 = ORIENTED_EDGE ( 'NONE', *, *, #13910, .T. ) ;
#4714 = DIRECTION ( 'NONE',  ( -0.8660254037844360431, -0.5000000000000045519, 0.000000000000000000 ) ) ;
#4715 = EDGE_CURVE ( 'NONE', #18333, #14531, #8447, .T. ) ;
#4716 = ORIENTED_EDGE ( 'NONE', *, *, #2526, .T. ) ;
#4717 = CARTESIAN_POINT ( 'NONE',  ( 209.1489059746362216, 31.20269758479947697, -12.34862215763092763 ) ) ;
#4718 = B_SPLINE_CURVE_WITH_KNOTS ( 'NONE', 3,
 ( #135, #236, #11577, #18047 ),
 .UNSPECIFIED., .F., .F.,
 ( 4, 4 ),
 ( 2.448070629215088117E-07, 0.0005857331628025484174 ),
 .UNSPECIFIED. ) ;
#4719 = DIRECTION ( 'NONE',  ( 0.000000000000000000, -0.000000000000000000, -1.000000000000000000 ) ) ;
#4720 = DIRECTION ( 'NONE',  ( -0.5000000000000041078, 0.8660254037844363761, 0.000000000000000000 ) ) ;
#4721 = CARTESIAN_POINT ( 'NONE',  ( 209.2115421631071968, 5.174237244332543284, -26.27710986211784672 ) ) ;
#4722 = CARTESIAN_POINT ( 'NONE',  ( -29.99999999999999645, 5.000000000000000000, -15.00000000000000000 ) ) ;
#4723 = EDGE_LOOP ( 'NONE', ( #16715, #12746, #10611, #13018, #5557, #15800 ) ) ;
#4724 = EDGE_CURVE ( 'NONE', #12607, #245, #916, .T. ) ;
#4725 = CARTESIAN_POINT ( 'NONE',  ( 197.6120640069452463, 5.208066731742445832, -21.80597602412970559 ) ) ;
#4726 = AXIS2_PLACEMENT_3D ( 'NONE', #2191, #15145, #18612 ) ;
#4727 = ORIENTED_EDGE ( 'NONE', *, *, #742, .F. ) ;
#4728 = DIRECTION ( 'NONE',  ( 0.5000000000000041078, -0.8660254037844362651, 0.000000000000000000 ) ) ;
#4729 = CARTESIAN_POINT ( 'NONE',  ( -10.39101401679802450, 49.56263860070575333, -11.18078835284466344 ) ) ;
#4730 = DIRECTION ( 'NONE',  ( -0.4895420438411626773, 0.8479116923739991041, -0.2034560130526446298 ) ) ;
#4731 = ADVANCED_FACE ( 'NONE', ( #11058 ), #7759, .T. ) ;
#4732 = AXIS2_PLACEMENT_3D ( 'NONE', #16765, #15309, #2352 ) ;
#4733 = DIRECTION ( 'NONE',  ( -0.5000000000000053291, 0.8660254037844354880, 0.000000000000000000 ) ) ;
#4734 = DIRECTION ( 'NONE',  ( -1.000000000000000000, 0.000000000000000000, 0.000000000000000000 ) ) ;
#4735 = ORIENTED_EDGE ( 'NONE', *, *, #20771, .F. ) ;
#4736 = ORIENTED_EDGE ( 'NONE', *, *, #8893, .F. ) ;
#4737 = CARTESIAN_POINT ( 'NONE',  ( 28.00000000000001066, 65.00000000000000000, -23.50000000000002842 ) ) ;
#4738 = CARTESIAN_POINT ( 'NONE',  ( 218.0493302439821548, 9.761530332989567071, -8.625373497621339425 ) ) ;
#4739 = EDGE_CURVE ( 'NONE', #16434, #2300, #4051, .T. ) ;
#4740 = CARTESIAN_POINT ( 'NONE',  ( -14.69985738491135052, 80.00000000000054001, -12.43489149392604887 ) ) ;
#4741 = EDGE_LOOP ( 'NONE', ( #7977, #18174 ) ) ;
#4742 = CARTESIAN_POINT ( 'NONE',  ( 229.4064455670339555, 36.39231742674856918, -12.92165662794199577 ) ) ;
#4743 = LINE ( 'NONE', #14634, #17661 ) ;
#4744 = CARTESIAN_POINT ( 'NONE',  ( 195.1526463715632076, 3.788121297904891271, -13.99656000852303173 ) ) ;
#4745 = COLOUR_RGB ( '',0.7921568627450980005, 0.8196078431372548767, 0.9333333333333333481 ) ;
#4746 = DIRECTION ( 'NONE',  ( 0.8660254037844355990, 0.5000000000000054401, 0.000000000000000000 ) ) ;
#4747 = ORIENTED_EDGE ( 'NONE', *, *, #13413, .F. ) ;
#4748 = AXIS2_PLACEMENT_3D ( 'NONE', #3225, #8517, #18270 ) ;
#4749 = VERTEX_POINT ( 'NONE', #17035 ) ;
#4750 = CARTESIAN_POINT ( 'NONE',  ( 30.00000000000000355, -9.999999999999998224, -15.00000000000000000 ) ) ;
#4751 = EDGE_CURVE ( 'NONE', #16239, #4535, #34, .T. ) ;
#4752 = EDGE_CURVE ( 'NONE', #9609, #5980, #9559, .T. ) ;
#4753 = CARTESIAN_POINT ( 'NONE',  ( 226.4416686084753110, 42.50692764314508310, -12.10162843130810373 ) ) ;
#4754 = CARTESIAN_POINT ( 'NONE',  ( 34.99529059433359635, 263.3427481158985870, -22.00000000000000355 ) ) ;
#4755 = CARTESIAN_POINT ( 'NONE',  ( -28.64932889238898284, 64.82996465168147893, 2.499044199174691450 ) ) ;
#4756 = CARTESIAN_POINT ( 'NONE',  ( 74.76692331049709139, 68.98407507634522062, -24.88169789286644118 ) ) ;
#4757 = AXIS2_PLACEMENT_3D ( 'NONE', #18142, #3612, #3204 ) ;
#4758 = EDGE_CURVE ( 'NONE', #17545, #20090, #19221, .T. ) ;
#4759 = CARTESIAN_POINT ( 'NONE',  ( -28.66754328919736849, 66.65723886915071716, 2.419320319690952292 ) ) ;
#4760 = VECTOR ( 'NONE', #17997, 1000.000000000000114 ) ;
#4761 = DIRECTION ( 'NONE',  ( 0.8660254037844348218, 0.5000000000000064393, 0.000000000000000000 ) ) ;
#4762 = CARTESIAN_POINT ( 'NONE',  ( 10.49211908931699178, 0.000000000000000000, -5.999999999999998224 ) ) ;
#4763 = ORIENTED_EDGE ( 'NONE', *, *, #3280, .T. ) ;
#4764 = CARTESIAN_POINT ( 'NONE',  ( 54.41450017449287913, 77.92833245222763594, -11.11271623845599699 ) ) ;
#4765 = VECTOR ( 'NONE', #5486, 1000.000000000000227 ) ;
#4766 = VERTEX_POINT ( 'NONE', #15462 ) ;
#4767 = EDGE_LOOP ( 'NONE', ( #13463, #4119, #8906, #5101 ) ) ;
#4768 = CARTESIAN_POINT ( 'NONE',  ( 1.064779251448269903, 73.59974835484908340, -0.1995438761926260351 ) ) ;
#4769 = EDGE_CURVE ( 'NONE', #5028, #2018, #3970, .T. ) ;
#4770 = AXIS2_PLACEMENT_3D ( 'NONE', #3868, #5657, #16709 ) ;
#4771 = CIRCLE ( 'NONE', #1721, 1.499999999999993783 ) ;
#4772 = FACE_OUTER_BOUND ( 'NONE', #6274, .T. ) ;
#4773 = APPLICATION_PROTOCOL_DEFINITION ( 'draft international standard', 'automotive_design', 1998, #2851 ) ;
#4774 = AXIS2_PLACEMENT_3D ( 'NONE', #16351, #18138, #14776 ) ;
#4775 = AXIS2_PLACEMENT_3D ( 'NONE', #6849, #5349, #18199 ) ;
#4776 = AXIS2_PLACEMENT_3D ( 'NONE', #17553, #4305, #6294 ) ;
#4777 = CARTESIAN_POINT ( 'NONE',  ( 216.3683575532814416, 33.19538101841234834, -14.00000000000004441 ) ) ;
#4778 = EDGE_LOOP ( 'NONE', ( #3662, #18094, #1260, #16661, #6660 ) ) ;
#4779 = CYLINDRICAL_SURFACE ( 'NONE', #6020, 4.999999999999997335 ) ;
#4780 = CARTESIAN_POINT ( 'NONE',  ( 218.5801281010350863, 37.63702161621608866, -16.29291827778579815 ) ) ;
#4781 = CARTESIAN_POINT ( 'NONE',  ( 208.8107687779841228, 4.427644383670616079, -14.00000000000005507 ) ) ;
#4782 = CARTESIAN_POINT ( 'NONE',  ( 0.000000000000000000, 4.685197434473812983, -6.938893903907228378E-15 ) ) ;
#4783 = CARTESIAN_POINT ( 'NONE',  ( 226.2172448981384036, 42.56917183590559972, -15.89588733937996601 ) ) ;
#4784 = DIRECTION ( 'NONE',  ( -1.000000000000000000, 0.000000000000000000, 0.000000000000000000 ) ) ;
#4785 = B_SPLINE_CURVE_WITH_KNOTS ( 'NONE', 3,
 ( #15419, #2681, #9024, #10719 ),
 .UNSPECIFIED., .F., .F.,
 ( 4, 4 ),
 ( 8.431164558841520529E-05, 0.0009382973835678675096 ),
 .UNSPECIFIED. ) ;
#4786 = DIRECTION ( 'NONE',  ( -0.7499999999999954481, -0.4330127018922224624, 0.5000000000000038858 ) ) ;
#4787 = VECTOR ( 'NONE', #16383, 1000.000000000000000 ) ;
#4788 = LINE ( 'NONE', #3400, #8571 ) ;
#4789 = CARTESIAN_POINT ( 'NONE',  ( 30.00000000000000355, 0.000000000000000000, -28.99999999999999645 ) ) ;
#4790 = ORIENTED_EDGE ( 'NONE', *, *, #12277, .T. ) ;
#4791 = AXIS2_PLACEMENT_3D ( 'NONE', #3360, #8119, #17901 ) ;
#4792 = CARTESIAN_POINT ( 'NONE',  ( 26.00000000000000355, 0.000000000000000000, 0.000000000000000000 ) ) ;
#4793 = DIRECTION ( 'NONE',  ( 1.000000000000000000, 0.000000000000000000, 0.000000000000000000 ) ) ;
#4794 = AXIS2_PLACEMENT_3D ( 'NONE', #8620, #8725, #7024 ) ;
#4795 = DIRECTION ( 'NONE',  ( 1.000000000000000000, 0.000000000000000000, 0.000000000000000000 ) ) ;
#4796 = DIRECTION ( 'NONE',  ( 0.000000000000000000, -1.000000000000000000, 0.000000000000000000 ) ) ;
#4797 = VECTOR ( 'NONE', #2819, 1000.000000000000114 ) ;
#4799 = ORIENTED_EDGE ( 'NONE', *, *, #9084, .T. ) ;
#4798 = ORIENTED_EDGE ( 'NONE', *, *, #4832, .T. ) ;
#4800 = CARTESIAN_POINT ( 'NONE',  ( -35.00000000000000000, 64.25000000000000000, -1.525597966176003961 ) ) ;
#4801 = CIRCLE ( 'NONE', #75, 11.00000000000002665 ) ;
#4802 = CARTESIAN_POINT ( 'NONE',  ( 219.6142080168453106, 10.66501293640096470, -14.00000000000005507 ) ) ;
#4803 = VERTEX_POINT ( 'NONE', #6265 ) ;
#4804 = FACE_OUTER_BOUND ( 'NONE', #9235, .T. ) ;
#4805 = ADVANCED_FACE ( 'NONE', ( #8062 ), #14570, .T. ) ;
#4806 = CARTESIAN_POINT ( 'NONE',  ( -30.24532165557386421, 79.23832348577512619, -7.772177369788165535 ) ) ;
#4807 = AXIS2_PLACEMENT_3D ( 'NONE', #1223, #20397, #16070 ) ;
#4808 = CARTESIAN_POINT ( 'NONE',  ( 215.5581897081276566, 15.56926723623108977, -18.15810777665862830 ) ) ;
#4809 = ORIENTED_EDGE ( 'NONE', *, *, #19845, .F. ) ;
#4810 = VECTOR ( 'NONE', #18113, 1000.000000000000114 ) ;
#4811 = CARTESIAN_POINT ( 'NONE',  ( 214.1694065045551838, 14.94446278398596206, -7.515250618841530894 ) ) ;
#4812 = DIRECTION ( 'NONE',  ( 0.8660254037844370423, 0.5000000000000026645, -0.000000000000000000 ) ) ;
#4813 = EDGE_CURVE ( 'NONE', #3474, #3214, #341, .T. ) ;
#4814 = CYLINDRICAL_SURFACE ( 'NONE', #1955, 5.000000000000005329 ) ;
#4815 = ORIENTED_EDGE ( 'NONE', *, *, #4581, .T. ) ;
#4816 = FACE_BOUND ( 'NONE', #18934, .T. ) ;
#4817 = CARTESIAN_POINT ( 'NONE',  ( 221.8667049707962633, 32.15042169561389329, -13.53966000285524096 ) ) ;
#4818 = ORIENTED_EDGE ( 'NONE', *, *, #16276, .F. ) ;
#4819 = FACE_OUTER_BOUND ( 'NONE', #15044, .T. ) ;
#4820 = CIRCLE ( 'NONE', #2470, 12.47473710546057823 ) ;
#4821 = PRESENTATION_LAYER_ASSIGNMENT (  '', '', ( #4502 ) ) ;
#4822 = ORIENTED_EDGE ( 'NONE', *, *, #12785, .T. ) ;
#4823 = DIRECTION ( 'NONE',  ( 0.5000000000000054401, -0.8660254037844354880, 0.000000000000000000 ) ) ;
#4824 = DIRECTION ( 'NONE',  ( -1.060575238724903217E-16, -6.123233995736827666E-17, 1.000000000000000000 ) ) ;
#4825 = DIRECTION ( 'NONE',  ( 0.8660254037844355990, 0.5000000000000054401, -8.899770914925154148E-15 ) ) ;
#4826 = EDGE_CURVE ( 'NONE', #11812, #9209, #15886, .T. ) ;
#4827 = CARTESIAN_POINT ( 'NONE',  ( 204.7255155853154918, 2.069022353175566931, -3.025685634606110952 ) ) ;
#4828 = FACE_OUTER_BOUND ( 'NONE', #14732, .T. ) ;
#4829 = ORIENTED_EDGE ( 'NONE', *, *, #1276, .T. ) ;
#4830 = CARTESIAN_POINT ( 'NONE',  ( 209.3941655698034197, 12.18747614486168906, -11.94626573465116692 ) ) ;
#4831 = VECTOR ( 'NONE', #15686, 1000.000000000000114 ) ;
#4832 = EDGE_CURVE ( 'NONE', #11067, #2925, #11682, .T. ) ;
#4833 = ORIENTED_EDGE ( 'NONE', *, *, #7680, .T. ) ;
#4834 = EDGE_CURVE ( 'NONE', #3652, #8582, #9790, .T. ) ;
#4835 = CARTESIAN_POINT ( 'NONE',  ( -4.309763885322762889, 45.97587668858208332, -4.475643294533367289 ) ) ;
#4836 = CARTESIAN_POINT ( 'NONE',  ( 229.1737920261087709, 37.77475107125530229, -11.32356490392481696 ) ) ;
#4837 = B_SPLINE_CURVE_WITH_KNOTS ( 'NONE', 3,
 ( #8928, #8717, #4166, #20166 ),
 .UNSPECIFIED., .F., .F.,
 ( 4, 4 ),
 ( 1.112364592875924249E-05, 0.0005770498682268473479 ),
 .UNSPECIFIED. ) ;
#4838 = CARTESIAN_POINT ( 'NONE',  ( 208.2336538649943236, 4.094446933302576142, -25.81526893633797570 ) ) ;
#4839 = CARTESIAN_POINT ( 'NONE',  ( -24.99005427693084158, 44.99862682014547488, -8.693708486900669996 ) ) ;
#4840 = EDGE_LOOP ( 'NONE', ( #9568, #10904, #6846, #9175 ) ) ;
#4841 = ORIENTED_EDGE ( 'NONE', *, *, #15272, .T. ) ;
#4842 = DIRECTION ( 'NONE',  ( -1.000000000000000000, 0.000000000000000000, 0.000000000000000000 ) ) ;
#4843 = DIRECTION ( 'NONE',  ( 0.5000000000000054401, -0.8660254037844354880, 0.000000000000000000 ) ) ;
#4844 = CARTESIAN_POINT ( 'NONE',  ( -13.92591801928538686, 79.99963191531476525, -12.37854261419849422 ) ) ;
#4845 = ORIENTED_EDGE ( 'NONE', *, *, #17940, .F. ) ;
#4846 = ORIENTED_EDGE ( 'NONE', *, *, #11460, .T. ) ;
#4847 = EDGE_CURVE ( 'NONE', #11315, #20129, #3485, .T. ) ;
#4848 = VERTEX_POINT ( 'NONE', #451 ) ;
#4849 = CARTESIAN_POINT ( 'NONE',  ( 5.000000000000004441, 2.342598717236856309, 4.057500000000020535 ) ) ;
#4850 = DIRECTION ( 'NONE',  ( 0.2961981327260292396, 0.1710100716628399076, 0.9396926207859056523 ) ) ;
#4851 = CARTESIAN_POINT ( 'NONE',  ( 195.0878360447208593, 3.573686361083222796, -14.00607376310509444 ) ) ;
#4852 = CARTESIAN_POINT ( 'NONE',  ( -11.70208324916672815, 63.89094914002017589, -2.555169535221542887 ) ) ;
#4853 = CONICAL_SURFACE ( 'NONE', #15035, 13.07248899748297433, 0.6693469023067423196 ) ;
#4854 = ORIENTED_EDGE ( 'NONE', *, *, #15000, .T. ) ;
#4855 = VERTEX_POINT ( 'NONE', #12972 ) ;
#4856 = LINE ( 'NONE', #5053, #2628 ) ;
#4857 = EDGE_CURVE ( 'NONE', #14093, #1146, #17943, .T. ) ;
#4858 = B_SPLINE_CURVE_WITH_KNOTS ( 'NONE', 3,
 ( #10623, #9342, #5850, #20483 ),
 .UNSPECIFIED., .F., .F.,
 ( 4, 4 ),
 ( 2.739824145226525125E-07, 0.0004523272241943725744 ),
 .UNSPECIFIED. ) ;
#4859 = PLANE ( 'NONE',  #13182 ) ;
#4860 = B_SPLINE_CURVE_WITH_KNOTS ( 'NONE', 3,
 ( #3304, #3610, #9752, #1714 ),
 .UNSPECIFIED., .F., .F.,
 ( 4, 4 ),
 ( 3.309335659841317687E-07, 0.0008543166715495293479 ),
 .UNSPECIFIED. ) ;
#4861 = ADVANCED_FACE ( 'NONE', ( #18147 ), #5095, .F. ) ;
#4862 = DIRECTION ( 'NONE',  ( 0.5000000000000042188, -0.8660254037844361541, -1.067522139062650425E-16 ) ) ;
#4863 = CARTESIAN_POINT ( 'NONE',  ( -32.09082692128702519, 61.27974766235208648, 2.035803694763616445 ) ) ;
#4864 = CARTESIAN_POINT ( 'NONE',  ( 45.00000000000000000, 5.000000000000000000, -15.00000000000000000 ) ) ;
#4865 = VECTOR ( 'NONE', #13704, 1000.000000000000114 ) ;
#4866 = VECTOR ( 'NONE', #13899, 1000.000000000000000 ) ;
#4867 = ORIENTED_EDGE ( 'NONE', *, *, #7845, .T. ) ;
#4868 = DIRECTION ( 'NONE',  ( -1.000000000000000000, -0.000000000000000000, -0.000000000000000000 ) ) ;
#4869 = CARTESIAN_POINT ( 'NONE',  ( 206.3904739784022695, 10.45329399600358400, -11.31442923650852883 ) ) ;
#4870 = EDGE_LOOP ( 'NONE', ( #2159, #5712, #10363, #14864 ) ) ;
#4871 = CARTESIAN_POINT ( 'NONE',  ( 56.48324548572979609, 77.04861762647422552, -7.597113510449146290 ) ) ;
#4872 = EDGE_CURVE ( 'NONE', #16648, #3315, #2037, .T. ) ;
#4873 = ORIENTED_EDGE ( 'NONE', *, *, #10149, .F. ) ;
#4874 = EDGE_CURVE ( 'NONE', #4395, #6174, #14240, .T. ) ;
#4875 = CARTESIAN_POINT ( 'NONE',  ( 208.0845375091750213, 4.265953788936775126, -1.899081834577966754 ) ) ;
#4876 = PLANE ( 'NONE',  #8300 ) ;
#4877 = CARTESIAN_POINT ( 'NONE',  ( 4.000000000000000000, 3.518949890710767026, -4.987329993433320396E-15 ) ) ;
#4878 = EDGE_LOOP ( 'NONE', ( #8295, #5480, #4488, #7388, #8574, #19725, #2282, #115, #15208, #11276, #13563, #16942, #13076, #12870, #3607, #15153, #12769, #3834, #16506, #8785, #18857, #7435, #8496, #9147, #14313, #19272, #8404, #17674, #11079, #6583, #12432, #12942, #2164, #17900, #2438, #15181, #15656, #17187, #6752, #6242, #16157, #17338, #4664, #93, #10034, #15328, #12823, #17369, #2789, #2915, #7851, #10620, #8043, #4939, #18621, #5539, #7890, #18015, #7382, #19720, #14845, #17896, #10005, #16635, #3987, #9118, #9041, #3354, #10778, #7603, #9369, #12679, #10100, #13665, #14935, #16656, #8007, #18832, #10868, #16504, #17473, #1357, #19589, #13705, #19911, #6312, #12968, #16627, #459, #4125, #7061, #18684 ) ) ;
#4879 = CARTESIAN_POINT ( 'NONE',  ( 220.2180084519553134, 35.41797800104779270, -14.00000000000005507 ) ) ;
#4880 = VERTEX_POINT ( 'NONE', #3614 ) ;
#4881 = VECTOR ( 'NONE', #16389, 1000.000000000000000 ) ;
#4882 = EDGE_CURVE ( 'NONE', #2539, #19041, #13377, .T. ) ;
#4883 = LINE ( 'NONE', #9742, #15383 ) ;
#4884 = ORIENTED_EDGE ( 'NONE', *, *, #6131, .T. ) ;
#4885 = FACE_OUTER_BOUND ( 'NONE', #516, .T. ) ;
#4886 = CARTESIAN_POINT ( 'NONE',  ( 210.1535261002520087, 29.22995462719417148, -16.48401562083277483 ) ) ;
#4887 = DIRECTION ( 'NONE',  ( -0.7500000000000014433, -0.4330127018922259596, -0.4999999999999919509 ) ) ;
#4888 = DIRECTION ( 'NONE',  ( 0.3841106397986906451, -0.6652991438591134843, 0.6401843996644803747 ) ) ;
#4889 = CARTESIAN_POINT ( 'NONE',  ( 211.2398691629905159, 12.72204434944011986, -24.79563718815145279 ) ) ;
#4890 = EDGE_CURVE ( 'NONE', #3590, #3527, #4718, .T. ) ;
#4891 = DIRECTION ( 'NONE',  ( 0.3886714912512188591, 0.2243995901002276971, -0.8936326403234180482 ) ) ;
#4892 = DIRECTION ( 'NONE',  ( 0.000000000000000000, -6.938893903907177533E-18, -1.000000000000000000 ) ) ;
#4893 = FACE_BOUND ( 'NONE', #3930, .T. ) ;
#4894 = EDGE_LOOP ( 'NONE', ( #11762, #6045, #20022 ) ) ;
#4895 = EDGE_LOOP ( 'NONE', ( #4845, #3011, #15915, #15122 ) ) ;
#4896 = FACE_BOUND ( 'NONE', #12073, .T. ) ;
#4897 = CARTESIAN_POINT ( 'NONE',  ( 59.03558430264390466, 85.14681185468893432, -10.05295229902272425 ) ) ;
#4898 = CARTESIAN_POINT ( 'NONE',  ( 217.6461549631789580, 37.74120415546371987, -16.68624095904335647 ) ) ;
#4899 = CARTESIAN_POINT ( 'NONE',  ( 80.10952826493171131, 51.56390520361809138, -19.09971892243163438 ) ) ;
#4901 = ORIENTED_EDGE ( 'NONE', *, *, #7247, .T. ) ;
#4900 = ORIENTED_EDGE ( 'NONE', *, *, #10765, .T. ) ;
#4902 = DIRECTION ( 'NONE',  ( 0.000000000000000000, 0.000000000000000000, -1.000000000000000000 ) ) ;
#4903 = UNCERTAINTY_MEASURE_WITH_UNIT (LENGTH_MEASURE( 1.000000000000000082E-05 ), #18366, 'distance_accuracy_value', 'NONE');
#4904 = CARTESIAN_POINT ( 'NONE',  ( 220.9434763298129951, 32.03007601957106232, -12.62147488791611671 ) ) ;
#4905 = ORIENTED_EDGE ( 'NONE', *, *, #20501, .F. ) ;
#4906 =( LENGTH_UNIT ( ) NAMED_UNIT ( * ) SI_UNIT ( .MILLI., .METRE. ) );
#4907 = CYLINDRICAL_SURFACE ( 'NONE', #13362, 5.000000000000005329 ) ;
#4908 = VECTOR ( 'NONE', #16601, 1000.000000000000227 ) ;
#4909 = LINE ( 'NONE', #3220, #12949 ) ;
#4910 = DIRECTION ( 'NONE',  ( 0.8660254037844360431, 0.5000000000000045519, 0.000000000000000000 ) ) ;
#4911 = DIRECTION ( 'NONE',  ( 0.5000000000000041078, -0.8660254037844363761, 0.000000000000000000 ) ) ;
#4912 = VERTEX_POINT ( 'NONE', #1935 ) ;
#4913 = DIRECTION ( 'NONE',  ( 0.000000000000000000, 6.938893903907178303E-18, 1.000000000000000000 ) ) ;
#4914 = DIRECTION ( 'NONE',  ( 1.000000000000000000, 0.000000000000000000, 0.000000000000000000 ) ) ;
#4915 = ORIENTED_EDGE ( 'NONE', *, *, #10307, .T. ) ;
#4916 = CARTESIAN_POINT ( 'NONE',  ( 207.8564944041415288, 11.29970128344166369, -11.99421842325719467 ) ) ;
#4917 = VERTEX_POINT ( 'NONE', #8382 ) ;
#4918 = CIRCLE ( 'NONE', #11363, 3.047499999999999876 ) ;
#4919 = DIRECTION ( 'NONE',  ( 0.000000000000000000, -0.4999999999999982792, 0.8660254037844395958 ) ) ;
#4920 = CARTESIAN_POINT ( 'NONE',  ( 209.3577037357181894, 3.480325248439694263, -14.00000000000005507 ) ) ;
#4921 = AXIS2_PLACEMENT_3D ( 'NONE', #16438, #11993, #440 ) ;
#4922 = CARTESIAN_POINT ( 'NONE',  ( 159.9952905943347901, 46.83639716978955647, -22.00000000000007816 ) ) ;
#4923 = CARTESIAN_POINT ( 'NONE',  ( 209.1177676012032407, 5.377710327540435209, -26.45271578590685380 ) ) ;
#4924 = EDGE_CURVE ( 'NONE', #9961, #402, #10066, .T. ) ;
#4925 = CARTESIAN_POINT ( 'NONE',  ( -28.38973003226371006, 8.717107242880045348, -1.690292246971881740 ) ) ;
#4926 = DIRECTION ( 'NONE',  ( -0.4895420438411641761, 0.8479116923740015466, 0.2034560130526309463 ) ) ;
#4927 = ORIENTED_EDGE ( 'NONE', *, *, #12269, .F. ) ;
#4928 = CARTESIAN_POINT ( 'NONE',  ( 77.72754490146294870, 67.46424320799033580, -25.26819846475408227 ) ) ;
#4929 = VECTOR ( 'NONE', #16279, 1000.000000000000227 ) ;
#4930 = CARTESIAN_POINT ( 'NONE',  ( 219.2109096010505311, 36.75039421051984334, -10.71100983847126642 ) ) ;
#4931 = ORIENTED_EDGE ( 'NONE', *, *, #11637, .T. ) ;
#4932 = CONICAL_SURFACE ( 'NONE', #12730, 13.07248899748297433, 0.6693469023067423196 ) ;
#4933 = DIRECTION ( 'NONE',  ( 0.000000000000000000, 6.938893903907178303E-18, 1.000000000000000000 ) ) ;
#4934 = CARTESIAN_POINT ( 'NONE',  ( -6.351643513575302435, 45.03196607589810441, -7.976803885185221432 ) ) ;
#4935 = CARTESIAN_POINT ( 'NONE',  ( -0.4023781907215778220, 78.75502016293279439, -6.506953707587063818 ) ) ;
#4936 = AXIS2_PLACEMENT_3D ( 'NONE', #12174, #9284, #732 ) ;
#4937 = DIRECTION ( 'NONE',  ( 0.5000000000000049960, -0.8660254037844357100, 0.000000000000000000 ) ) ;
#4938 = CARTESIAN_POINT ( 'NONE',  ( -23.23502873769109556, 45.07676717092099494, -10.20065155966471337 ) ) ;
#4940 = EDGE_LOOP ( 'NONE', ( #13072, #790, #9800, #18970, #1604 ) ) ;
#4939 = ORIENTED_EDGE ( 'NONE', *, *, #6732, .T. ) ;
#4941 = VERTEX_POINT ( 'NONE', #654 ) ;
#4942 = EDGE_LOOP ( 'NONE', ( #20506, #4798, #16031, #4357, #20535 ) ) ;
#4943 = FACE_OUTER_BOUND ( 'NONE', #14265, .T. ) ;
#4944 = DIRECTION ( 'NONE',  ( 0.8660254037844372643, 0.5000000000000027756, -0.000000000000000000 ) ) ;
#4945 = ORIENTED_EDGE ( 'NONE', *, *, #5947, .T. ) ;
#4946 = ORIENTED_EDGE ( 'NONE', *, *, #2830, .T. ) ;
#4947 = CARTESIAN_POINT ( 'NONE',  ( -18.57020691453844208, 59.27322340592550631, -4.297493274131830354 ) ) ;
#4948 = DIRECTION ( 'NONE',  ( -0.5000000000000029976, 0.8660254037844370423, 0.000000000000000000 ) ) ;
#4949 = CARTESIAN_POINT ( 'NONE',  ( 226.2066167028222594, 42.91404948615199544, -14.93232347545819216 ) ) ;
#4950 = AXIS2_PLACEMENT_3D ( 'NONE', #18786, #5719, #4039 ) ;
#4951 = CARTESIAN_POINT ( 'NONE',  ( 218.1839418517603235, 38.32323632922017254, -14.53509620734043217 ) ) ;
#4952 = EDGE_LOOP ( 'NONE', ( #13127, #11573, #8046, #15523 ) ) ;
#4953 = EDGE_CURVE ( 'NONE', #1656, #8535, #13488, .T. ) ;
#4954 = ORIENTED_EDGE ( 'NONE', *, *, #3336, .F. ) ;
#4955 = AXIS2_PLACEMENT_3D ( 'NONE', #14187, #19050, #17453 ) ;
#4956 = EDGE_CURVE ( 'NONE', #10290, #19333, #8811, .T. ) ;
#4957 = CARTESIAN_POINT ( 'NONE',  ( 157.3972143829815309, 45.33639716978957068, -22.00000000000007816 ) ) ;
#4958 = DIRECTION ( 'NONE',  ( -0.5000000000000008882, 0.8660254037844381525, 0.000000000000000000 ) ) ;
#4959 = CARTESIAN_POINT ( 'NONE',  ( 216.6640881527418401, 8.961760438719156951, -23.53124788243930610 ) ) ;
#4960 = CARTESIAN_POINT ( 'NONE',  ( 200.0157312721003393, 23.75418783301503467, -14.00000000000005507 ) ) ;
#4961 = LINE ( 'NONE', #108, #10236 ) ;
#4962 = PLANE ( 'NONE',  #926 ) ;
#4963 = CARTESIAN_POINT ( 'NONE',  ( 27.00000000000002487, 65.74999999999997158, 2.481238266578629226 ) ) ;
#4964 = CIRCLE ( 'NONE', #4297, 1.499999999999990896 ) ;
#4965 = VERTEX_POINT ( 'NONE', #8914 ) ;
#4966 = ORIENTED_EDGE ( 'NONE', *, *, #358, .T. ) ;
#4968 = EDGE_CURVE ( 'NONE', #20000, #18033, #338, .T. ) ;
#4967 = CARTESIAN_POINT ( 'NONE',  ( 59.47135335676293977, 84.81187091046737692, -9.105437536888221217 ) ) ;
#4969 = VERTEX_POINT ( 'NONE', #4154 ) ;
#4970 = DIRECTION ( 'NONE',  ( 0.5566703992264088185, 0.3213938048432679051, -0.7660444431189864511 ) ) ;
#4971 = PLANE ( 'NONE',  #14789 ) ;
#4972 = EDGE_CURVE ( 'NONE', #19075, #6984, #13700, .T. ) ;
#4973 = ORIENTED_EDGE ( 'NONE', *, *, #6796, .F. ) ;
#4974 = CARTESIAN_POINT ( 'NONE',  ( 226.6332897176000074, 42.17503014633813052, -11.12998660979000931 ) ) ;
#4975 = EDGE_CURVE ( 'NONE', #8807, #20547, #11855, .T. ) ;
#4976 = CARTESIAN_POINT ( 'NONE',  ( 44.05523633727993627, 164.6504617752990498, -12.50000000000000000 ) ) ;
#4977 = ORIENTED_EDGE ( 'NONE', *, *, #12310, .F. ) ;
#4978 = ADVANCED_FACE ( 'NONE', ( #15514 ), #7417, .F. ) ;
#4979 = DIRECTION ( 'NONE',  ( 0.000000000000000000, -1.000000000000000000, 0.000000000000000000 ) ) ;
#4980 = CARTESIAN_POINT ( 'NONE',  ( 177.1791022559528983, 56.75747545832872731, -14.00000000000006395 ) ) ;
#4981 = VECTOR ( 'NONE', #11076, 1000.000000000000227 ) ;
#4982 = ADVANCED_FACE ( 'NONE', ( #13906 ), #12101, .T. ) ;
#4983 = DIRECTION ( 'NONE',  ( -0.8660254037844361541, -0.5000000000000045519, 5.976026924694053325E-17 ) ) ;
#4984 = CARTESIAN_POINT ( 'NONE',  ( 28.00000000000001066, 65.00000000000000000, -12.50000000000000000 ) ) ;
#4985 = LINE ( 'NONE', #12966, #15714 ) ;
#4986 = DIRECTION ( 'NONE',  ( -0.000000000000000000, -0.000000000000000000, 1.000000000000000000 ) ) ;
#4987 = VERTEX_POINT ( 'NONE', #13597 ) ;
#4989 = ADVANCED_FACE ( 'NONE', ( #20052 ), #10146, .T. ) ;
#4988 = FACE_OUTER_BOUND ( 'NONE', #13675, .T. ) ;
#4990 = CARTESIAN_POINT ( 'NONE',  ( 58.64832549623106672, 85.44433982373099923, -11.49787480049970334 ) ) ;
#4991 = CIRCLE ( 'NONE', #12794, 3.902363844300875240 ) ;
#4992 = CARTESIAN_POINT ( 'NONE',  ( 227.5312376355471145, 39.64027283883993391, -14.00000000000005507 ) ) ;
#4993 = CARTESIAN_POINT ( 'NONE',  ( 78.65134511289586783, 53.39203929102664858, -18.47032050442678397 ) ) ;
#4994 = VECTOR ( 'NONE', #4343, 1000.000000000000227 ) ;
#4995 = ORIENTED_EDGE ( 'NONE', *, *, #14078, .F. ) ;
#4996 = VERTEX_POINT ( 'NONE', #18676 ) ;
#4997 = EDGE_CURVE ( 'NONE', #11555, #17136, #5615, .T. ) ;
#4998 = EDGE_CURVE ( 'NONE', #18930, #12331, #15610, .T. ) ;
#4999 = FACE_OUTER_BOUND ( 'NONE', #2090, .T. ) ;
#5000 = EDGE_LOOP ( 'NONE', ( #2473, #17932, #3278, #19368, #13783, #6281 ) ) ;
#5001 = FILL_AREA_STYLE_COLOUR ( '', #3310 ) ;
#5002 = CARTESIAN_POINT ( 'NONE',  ( -27.98085110631299344, 80.00000000015971580, -3.582299587997329837 ) ) ;
#5003 = CARTESIAN_POINT ( 'NONE',  ( 4.000000000000000000, -3.518949890710766581, 4.553649124439118623E-15 ) ) ;
#5004 = EDGE_CURVE ( 'NONE', #6727, #8661, #2463, .T. ) ;
#5005 = VECTOR ( 'NONE', #14351, 1000.000000000000114 ) ;
#5006 = VECTOR ( 'NONE', #7101, 1000.000000000000000 ) ;
#5007 = CARTESIAN_POINT ( 'NONE',  ( 195.2378745322255611, 8.138335620992030783, -7.515250618841283092 ) ) ;
#5008 = AXIS2_PLACEMENT_3D ( 'NONE', #7460, #10745, #18817 ) ;
#5009 = EDGE_CURVE ( 'NONE', #340, #791, #18570, .T. ) ;
#5010 = CARTESIAN_POINT ( 'NONE',  ( 213.5545353545354601, 14.58946676000514486, -21.69368824361360382 ) ) ;
#5011 = DIRECTION ( 'NONE',  ( -0.5000000000000045519, 0.8660254037844360431, 0.000000000000000000 ) ) ;
#5012 = ORIENTED_EDGE ( 'NONE', *, *, #7026, .F. ) ;
#5014 = EDGE_CURVE ( 'NONE', #784, #19322, #12224, .T. ) ;
#5013 = SURFACE_STYLE_FILL_AREA ( #2167 ) ;
#5015 = DIRECTION ( 'NONE',  ( -0.5000000000000054401, 0.8660254037844354880, -0.000000000000000000 ) ) ;
#5016 = ORIENTED_EDGE ( 'NONE', *, *, #14063, .T. ) ;
#5017 = CARTESIAN_POINT ( 'NONE',  ( -14.99999999999999645, 5.000000000000000000, 15.00000000000000000 ) ) ;
#5018 = ORIENTED_EDGE ( 'NONE', *, *, #18328, .T. ) ;
#5019 = VECTOR ( 'NONE', #6472, 1000.000000000000000 ) ;
#5020 = DIRECTION ( 'NONE',  ( -0.7235536692358585098, -0.4177439057064706307, 0.5495089780708131144 ) ) ;
#5021 = FACE_BOUND ( 'NONE', #3411, .T. ) ;
#5022 = DIRECTION ( 'NONE',  ( -0.8660254037844361541, -0.5000000000000045519, -8.850264995343378780E-15 ) ) ;
#5023 = EDGE_CURVE ( 'NONE', #3344, #13130, #2570, .T. ) ;
#5024 = PRODUCT_DEFINITION_FORMATION_WITH_SPECIFIED_SOURCE ( 'ANY', '', #12121, .NOT_KNOWN. ) ;
#5025 = FACE_OUTER_BOUND ( 'NONE', #9923, .T. ) ;
#5026 = CARTESIAN_POINT ( 'NONE',  ( 32.39721438298032297, 261.8427481158985870, -22.00000000000000355 ) ) ;
#5027 = DIRECTION ( 'NONE',  ( -0.8660254037844355990, -0.5000000000000054401, 0.000000000000000000 ) ) ;
#5028 = VERTEX_POINT ( 'NONE', #9015 ) ;
#5029 = CARTESIAN_POINT ( 'NONE',  ( 71.93434708225751706, 72.55958424763308301, -23.26416705100350768 ) ) ;
#5030 = DIRECTION ( 'NONE',  ( 0.8660254037844374864, 0.5000000000000021094, 2.220446049250313081E-16 ) ) ;
#5031 = VECTOR ( 'NONE', #17076, 1000.000000000000227 ) ;
#5032 = VERTEX_POINT ( 'NONE', #16980 ) ;
#5033 =( NAMED_UNIT ( * ) SI_UNIT ( $, .STERADIAN. ) SOLID_ANGLE_UNIT ( ) );
#5034 = CARTESIAN_POINT ( 'NONE',  ( -3.616241391857264009, 47.72147621156500463, -1.725877097790484704 ) ) ;
#5035 = DIRECTION ( 'NONE',  ( -0.5000000000000054401, 0.8660254037844354880, -0.000000000000000000 ) ) ;
#5036 = DIRECTION ( 'NONE',  ( -0.8660254037844363761, -0.5000000000000043299, 6.872020471724002955E-17 ) ) ;
#5037 = CARTESIAN_POINT ( 'NONE',  ( 226.6211368133091923, 39.11482588413117867, -14.00000000000005507 ) ) ;
#5038 = ADVANCED_FACE ( 'NONE', ( #10276 ), #15411, .F. ) ;
#5039 = ORIENTED_EDGE ( 'NONE', *, *, #16901, .F. ) ;
#5040 = ORIENTED_EDGE ( 'NONE', *, *, #19252, .T. ) ;
#5041 = ORIENTED_EDGE ( 'NONE', *, *, #12902, .T. ) ;
#5042 = CARTESIAN_POINT ( 'NONE',  ( 201.4983898220421850, 0.4634396488479761711, -22.82042918318446212 ) ) ;
#5043 = DIRECTION ( 'NONE',  ( 1.000000000000000000, 0.000000000000000000, 0.000000000000000000 ) ) ;
#5044 = VERTEX_POINT ( 'NONE', #17189 ) ;
#5045 = EDGE_LOOP ( 'NONE', ( #20045, #3314, #3913 ) ) ;
#5046 = DIRECTION ( 'NONE',  ( 0.5000000000000007772, -0.8660254037844381525, 0.000000000000000000 ) ) ;
#5047 = DIRECTION ( 'NONE',  ( 0.8660254037844370423, 0.5000000000000026645, -0.000000000000000000 ) ) ;
#5048 = DIRECTION ( 'NONE',  ( 1.000000000000000000, -0.000000000000000000, -0.000000000000000000 ) ) ;
#5049 = CARTESIAN_POINT ( 'NONE',  ( 201.9167561165444056, 0.4473843177916839164, -14.00000000000005507 ) ) ;
#5050 = ORIENTED_EDGE ( 'NONE', *, *, #2121, .T. ) ;
#5051 = AXIS2_PLACEMENT_3D ( 'NONE', #18943, #12696, #2839 ) ;
#5052 = ORIENTED_EDGE ( 'NONE', *, *, #8061, .T. ) ;
#5053 = CARTESIAN_POINT ( 'NONE',  ( 227.2053588074475670, 41.18417741728240600, -14.00000000000005507 ) ) ;
#5054 = EDGE_CURVE ( 'NONE', #15623, #9666, #12844, .T. ) ;
#5055 = B_SPLINE_CURVE_WITH_KNOTS ( 'NONE', 3,
 ( #9390, #18853, #12704, #1157 ),
 .UNSPECIFIED., .F., .F.,
 ( 4, 4 ),
 ( 2.764878223179000381E-07, 0.0004523297296022163829 ),
 .UNSPECIFIED. ) ;
#5056 = DIRECTION ( 'NONE',  ( 0.8660254037844360431, 0.5000000000000045519, -0.000000000000000000 ) ) ;
#5057 = TOROIDAL_SURFACE ( 'NONE', #15577, 5.400000000000001243, 0.4000000000000000222 ) ;
#5058 = CARTESIAN_POINT ( 'NONE',  ( 5.000000000000004441, 3.513898075855356407, -2.028750000000020481 ) ) ;
#5059 = CARTESIAN_POINT ( 'NONE',  ( -32.38649895722338812, 50.74460817506653143, -7.785217389867390203 ) ) ;
#5060 = CARTESIAN_POINT ( 'NONE',  ( 208.0983737146324870, 5.661548828456886895, -14.00000000000005507 ) ) ;
#5061 = ORIENTED_EDGE ( 'NONE', *, *, #7329, .F. ) ;
#5062 = DIRECTION ( 'NONE',  ( 0.5000000000000044409, -0.8660254037844361541, 0.000000000000000000 ) ) ;
#5063 = VECTOR ( 'NONE', #8503, 1000.000000000000000 ) ;
#5064 = DIRECTION ( 'NONE',  ( 0.8660254037844380415, 0.5000000000000014433, 0.000000000000000000 ) ) ;
#5065 = ADVANCED_FACE ( 'NONE', ( #12840 ), #15821, .F. ) ;
#5066 = VERTEX_POINT ( 'NONE', #1292 ) ;
#5067 = AXIS2_PLACEMENT_3D ( 'NONE', #1954, #9779, #14699 ) ;
#5068 = CARTESIAN_POINT ( 'NONE',  ( 62.81266095603159272, 74.33819947169733666, -3.428479281352090347 ) ) ;
#5069 = AXIS2_PLACEMENT_3D ( 'NONE', #8542, #6940, #700 ) ;
#5070 = ORIENTED_EDGE ( 'NONE', *, *, #10706, .T. ) ;
#5071 = FACE_OUTER_BOUND ( 'NONE', #16818, .T. ) ;
#5072 = DIRECTION ( 'NONE',  ( -0.5000000000000049960, 0.8660254037844358210, -0.000000000000000000 ) ) ;
#5073 = ORIENTED_EDGE ( 'NONE', *, *, #18487, .T. ) ;
#5074 = LINE ( 'NONE', #9941, #17848 ) ;
#5075 = AXIS2_PLACEMENT_3D ( 'NONE', #11592, #2258, #15212 ) ;
#5076 = DIRECTION ( 'NONE',  ( 0.5000000000000046629, -0.8660254037844360431, -4.006172263299081054E-16 ) ) ;
#5077 = EDGE_LOOP ( 'NONE', ( #10295, #3158, #12362, #12866 ) ) ;
#5078 = VECTOR ( 'NONE', #20271, 1000.000000000000114 ) ;
#5079 = DIRECTION ( 'NONE',  ( -1.000000000000000000, 0.000000000000000000, 0.000000000000000000 ) ) ;
#5080 = DIRECTION ( 'NONE',  ( 0.8660254037844355990, 0.5000000000000054401, 0.000000000000000000 ) ) ;
#5081 = AXIS2_PLACEMENT_3D ( 'NONE', #16688, #8723, #12023 ) ;
#5082 = CARTESIAN_POINT ( 'NONE',  ( 22.00490953756709800, 255.8427481158984733, 1.000000000000028644 ) ) ;
#5083 = CARTESIAN_POINT ( 'NONE',  ( 191.5478494775925640, 36.18576207517880050, -14.00000000000006395 ) ) ;
#5084 = TOROIDAL_SURFACE ( 'NONE', #3398, 6.500000000000000888, 1.500000000000000000 ) ;
#5085 = EDGE_CURVE ( 'NONE', #11761, #15457, #19196, .T. ) ;
#5086 = VERTEX_POINT ( 'NONE', #17294 ) ;
#5087 = CARTESIAN_POINT ( 'NONE',  ( 43.39721438298041534, 242.7901892326410120, -13.99999999999998046 ) ) ;
#5088 = PLANE ( 'NONE',  #11301 ) ;
#5089 = DIRECTION ( 'NONE',  ( 0.7739085681710395903, 0.4468163201617135760, 0.4487991802004505648 ) ) ;
#5090 = EDGE_CURVE ( 'NONE', #16824, #14795, #15723, .T. ) ;
#5091 = ORIENTED_EDGE ( 'NONE', *, *, #6283, .T. ) ;
#5092 = CARTESIAN_POINT ( 'NONE',  ( 200.4364383576235866, 6.484680665789935183, -3.188775577416750995 ) ) ;
#5093 = CARTESIAN_POINT ( 'NONE',  ( 63.30970132782791637, 81.85394346738576132, -4.971994580379090145 ) ) ;
#5094 = AXIS2_PLACEMENT_3D ( 'NONE', #14839, #11525, #17584 ) ;
#5095 = PLANE ( 'NONE',  #11498 ) ;
#5096 = CARTESIAN_POINT ( 'NONE',  ( 75.33920648802740061, 52.40915241012807968, -9.253810560353768366 ) ) ;
#5097 = ORIENTED_EDGE ( 'NONE', *, *, #3830, .T. ) ;
#5098 = ORIENTED_EDGE ( 'NONE', *, *, #15669, .F. ) ;
#5099 = AXIS2_PLACEMENT_3D ( 'NONE', #1983, #9910, #8431 ) ;
#5100 = ADVANCED_FACE ( 'NONE', ( #20870 ), #13688, .F. ) ;
#5101 = ORIENTED_EDGE ( 'NONE', *, *, #6789, .T. ) ;
#5102 = ORIENTED_EDGE ( 'NONE', *, *, #3972, .T. ) ;
#5103 = DIRECTION ( 'NONE',  ( -1.000000000000000000, -0.000000000000000000, -0.000000000000000000 ) ) ;
#5104 = ORIENTED_EDGE ( 'NONE', *, *, #5853, .F. ) ;
#5105 = CARTESIAN_POINT ( 'NONE',  ( 10.49211908931699178, 0.000000000000000000, -5.999999999999998224 ) ) ;
#5106 = PLANE ( 'NONE',  #9300 ) ;
#5107 = DIRECTION ( 'NONE',  ( -0.5000000000000049960, 0.8660254037844358210, -0.000000000000000000 ) ) ;
#5108 = EDGE_CURVE ( 'NONE', #16512, #255, #5449, .T. ) ;
#5109 = VECTOR ( 'NONE', #5124, 1000.000000000000000 ) ;
#5110 = CARTESIAN_POINT ( 'NONE',  ( 209.4254563108873413, 4.782534396259779719, -2.187257959407755248 ) ) ;
#5111 = AXIS2_PLACEMENT_3D ( 'NONE', #9397, #2645, #20538 ) ;
#5112 = EDGE_CURVE ( 'NONE', #1455, #13549, #11532, .T. ) ;
#5113 = VECTOR ( 'NONE', #7472, 1000.000000000000000 ) ;
#5114 = CARTESIAN_POINT ( 'NONE',  ( 54.49397420869091491, 77.89457764545490193, -14.16833317594359798 ) ) ;
#5115 = CARTESIAN_POINT ( 'NONE',  ( 188.6991442264338446, 14.97787164915609104, -11.13829696442576811 ) ) ;
#5116 = ORIENTED_EDGE ( 'NONE', *, *, #13957, .F. ) ;
#5117 = LINE ( 'NONE', #6815, #7779 ) ;
#5118 = CARTESIAN_POINT ( 'NONE',  ( 188.9132435853528591, 28.89116896218935082, -14.00000000000004086 ) ) ;
#5119 = CARTESIAN_POINT ( 'NONE',  ( 30.00000000000000000, 5.000000000000000000, 15.00000000000000000 ) ) ;
#5120 = ADVANCED_FACE ( 'NONE', ( #10041 ), #11200, .T. ) ;
#5121 = EDGE_LOOP ( 'NONE', ( #18026, #14518, #5347 ) ) ;
#5122 = EDGE_CURVE ( 'NONE', #18502, #8117, #19612, .T. ) ;
#5123 = DIRECTION ( 'NONE',  ( 0.000000000000000000, 0.8660254037844395958, 0.4999999999999982792 ) ) ;
#5124 = DIRECTION ( 'NONE',  ( 0.8426815769442658199, 0.4865224352899167326, -0.2306158707424411092 ) ) ;
#5125 = CARTESIAN_POINT ( 'NONE',  ( 219.1667714839435632, 10.92189157256192900, -15.42246552719623587 ) ) ;
#5126 = CONICAL_SURFACE ( 'NONE', #16995, 10.85470691220533190, 0.8171114040043576665 ) ;
#5127 = AXIS2_PLACEMENT_3D ( 'NONE', #4348, #17493, #10800 ) ;
#5128 = CARTESIAN_POINT ( 'NONE',  ( 43.00000000000000000, 0.000000000000000000, 3.309499999999999886 ) ) ;
#5129 = CARTESIAN_POINT ( 'NONE',  ( -27.41869751006752409, 6.332780952808748864, -5.130582469439492144 ) ) ;
#5130 = DIRECTION ( 'NONE',  ( 0.9885408208161367005, 0.000000000000000000, -0.1509537862398905028 ) ) ;
#5131 = EDGE_CURVE ( 'NONE', #4941, #4987, #8360, .T. ) ;
#5132 = ORIENTED_EDGE ( 'NONE', *, *, #5112, .T. ) ;
#5133 = CARTESIAN_POINT ( 'NONE',  ( 73.03466427698670316, 69.80725080074495281, -24.59324696420904033 ) ) ;
#5134 = CARTESIAN_POINT ( 'NONE',  ( -3.528418202498509348, 50.52477872402794645, 0.9493153023570927163 ) ) ;
#5135 = ORIENTED_EDGE ( 'NONE', *, *, #13192, .T. ) ;
#5136 = PLANE ( 'NONE',  #20393 ) ;
#5137 = CARTESIAN_POINT ( 'NONE',  ( -3.989626255526430132, 52.36474351664826798, -4.388076984466315444 ) ) ;
#5138 = CARTESIAN_POINT ( 'NONE',  ( 159.9952905943347901, 46.83639716978954226, -6.000000000000052403 ) ) ;
#5139 = EDGE_CURVE ( 'NONE', #17374, #20019, #2707, .T. ) ;
#5140 = VECTOR ( 'NONE', #1303, 1000.000000000000000 ) ;
#5141 = FACE_OUTER_BOUND ( 'NONE', #181, .T. ) ;
#5142 = DIRECTION ( 'NONE',  ( -0.6518835024542816159, 0.000000000000000000, 0.7583191275630192241 ) ) ;
#5143 = CIRCLE ( 'NONE', #2460, 1.003313105759049417 ) ;
#5144 = LINE ( 'NONE', #13534, #16096 ) ;
#5146 = ORIENTED_EDGE ( 'NONE', *, *, #319, .T. ) ;
#5145 = ORIENTED_EDGE ( 'NONE', *, *, #15109, .T. ) ;
#5147 = ORIENTED_EDGE ( 'NONE', *, *, #14759, .F. ) ;
#5148 = CARTESIAN_POINT ( 'NONE',  ( 215.9755601355957424, 15.98724606906508683, -13.98704593443257771 ) ) ;
#5149 = CARTESIAN_POINT ( 'NONE',  ( 200.3972727712213668, 6.993117665730062882, -3.627429155984474907 ) ) ;
#5150 = VERTEX_POINT ( 'NONE', #16533 ) ;
#5151 = ORIENTED_EDGE ( 'NONE', *, *, #2830, .F. ) ;
#5152 = CARTESIAN_POINT ( 'NONE',  ( -18.30650389616927498, 59.06684029410003234, -4.447567583327522556 ) ) ;
#5153 = CARTESIAN_POINT ( 'NONE',  ( 220.0716363630204739, 35.67150189589299458, -10.10863206319040941 ) ) ;
#5154 = CARTESIAN_POINT ( 'NONE',  ( 9.999999999999994671, 0.000000000000000000, 0.000000000000000000 ) ) ;
#5155 = CARTESIAN_POINT ( 'NONE',  ( -12.78406828249000782, 59.99816190035672747, -3.834978693179208697 ) ) ;
#5156 = ORIENTED_EDGE ( 'NONE', *, *, #6571, .T. ) ;
#5157 = VERTEX_POINT ( 'NONE', #3380 ) ;
#5158 = CARTESIAN_POINT ( 'NONE',  ( 208.4761278624580711, 5.007259451653140125, -14.00000000000005507 ) ) ;
#5159 = CIRCLE ( 'NONE', #20737, 5.999999999999998224 ) ;
#5160 = CARTESIAN_POINT ( 'NONE',  ( 227.6676214618444476, 40.05704593745944919, -10.29768792660754073 ) ) ;
#5161 = DIRECTION ( 'NONE',  ( 1.000000000000000000, 0.000000000000000000, -1.051300182579813185E-16 ) ) ;
#5162 = CARTESIAN_POINT ( 'NONE',  ( -28.94833220779161920, 56.54499750659159929, -0.09259939256140287123 ) ) ;
#5163 = CARTESIAN_POINT ( 'NONE',  ( -31.74999999999995737, 0.000000000000000000, 0.000000000000000000 ) ) ;
#5164 = EDGE_LOOP ( 'NONE', ( #19040, #1390, #998, #1524 ) ) ;
#5165 = CARTESIAN_POINT ( 'NONE',  ( 210.6089461623840009, 5.465822580604545955, -25.65046807331635748 ) ) ;
#5166 = CARTESIAN_POINT ( 'NONE',  ( 93.04593889385130012, 210.2557651598135351, 11.00000000000000888 ) ) ;
#5167 = ORIENTED_EDGE ( 'NONE', *, *, #14381, .T. ) ;
#5168 = VECTOR ( 'NONE', #757, 1000.000000000000000 ) ;
#5169 = CARTESIAN_POINT ( 'NONE',  ( 62.23039322790586425, 78.39221673943322344, -10.60002489424368122 ) ) ;
#5170 = ORIENTED_EDGE ( 'NONE', *, *, #7845, .F. ) ;
#5171 = ORIENTED_EDGE ( 'NONE', *, *, #9282, .F. ) ;
#5172 = VERTEX_POINT ( 'NONE', #9835 ) ;
#5173 = CARTESIAN_POINT ( 'NONE',  ( 226.6218208878421194, 41.21542885111893639, -17.45257705044830843 ) ) ;
#5174 = DIRECTION ( 'NONE',  ( -1.000000000000000000, 0.000000000000000000, -0.000000000000000000 ) ) ;
#5175 = ORIENTED_EDGE ( 'NONE', *, *, #13805, .F. ) ;
#5176 = LINE ( 'NONE', #6656, #9693 ) ;
#5177 = ORIENTED_EDGE ( 'NONE', *, *, #15347, .F. ) ;
#5178 = CARTESIAN_POINT ( 'NONE',  ( 218.1033169702945997, 10.30790582283579759, -19.52417598135495425 ) ) ;
#5179 = ORIENTED_EDGE ( 'NONE', *, *, #7076, .F. ) ;
#5180 = ADVANCED_FACE ( 'NONE', ( #5071 ), #5084, .T. ) ;
#5181 = AXIS2_PLACEMENT_3D ( 'NONE', #11039, #13055, #9430 ) ;
#5182 = CARTESIAN_POINT ( 'NONE',  ( 227.1116836665104302, 41.34642752079204087, -17.14987233279964585 ) ) ;
#5183 = VECTOR ( 'NONE', #14256, 1000.000000000000114 ) ;
#5184 = CARTESIAN_POINT ( 'NONE',  ( 218.8959393621077254, 37.70786883578019655, -11.12998660979001286 ) ) ;
#5185 = FACE_OUTER_BOUND ( 'NONE', #16023, .T. ) ;
#5186 = PLANE ( 'NONE',  #3478 ) ;
#5187 = VERTEX_POINT ( 'NONE', #5173 ) ;
#5188 = DIRECTION ( 'NONE',  ( -0.8137976813493728034, -0.4698463103929603757, -0.3420201433256622736 ) ) ;
#5189 = CARTESIAN_POINT ( 'NONE',  ( 30.10683012259193703, 0.000000000000000000, -5.999999999999998224 ) ) ;
#5190 = CARTESIAN_POINT ( 'NONE',  ( 198.5343390728978932, -1.505455072869313238, -12.62839849932143643 ) ) ;
#5191 = ORIENTED_EDGE ( 'NONE', *, *, #13634, .T. ) ;
#5192 = CARTESIAN_POINT ( 'NONE',  ( 215.9194406937061217, 8.531838027793467560, -5.321846656828220112 ) ) ;
#5193 = CARTESIAN_POINT ( 'NONE',  ( 202.2752485137783083, 25.28694651298519958, -12.50009056643368943 ) ) ;
#5194 = EDGE_LOOP ( 'NONE', ( #17429, #19662, #14129, #16958 ) ) ;
#5195 = CARTESIAN_POINT ( 'NONE',  ( -14.12934535402923153, 71.18264261159711737, -4.639596491434939907 ) ) ;
#5196 = CARTESIAN_POINT ( 'NONE',  ( 80.47222577874747174, 52.59073085207923270, -20.35369553621190519 ) ) ;
#5198 = ORIENTED_EDGE ( 'NONE', *, *, #9866, .T. ) ;
#5197 = ORIENTED_EDGE ( 'NONE', *, *, #16779, .T. ) ;
#5199 = ORIENTED_EDGE ( 'NONE', *, *, #1376, .T. ) ;
#5200 = VERTEX_POINT ( 'NONE', #12946 ) ;
#5201 = EDGE_CURVE ( 'NONE', #566, #13651, #12050, .T. ) ;
#5202 = FACE_OUTER_BOUND ( 'NONE', #14623, .T. ) ;
#5203 = ORIENTED_EDGE ( 'NONE', *, *, #1995, .T. ) ;
#5204 = CARTESIAN_POINT ( 'NONE',  ( 75.64423735160997353, 52.81473335711799422, -17.04225810597251467 ) ) ;
#5205 = EDGE_CURVE ( 'NONE', #9631, #19907, #2734, .T. ) ;
#5206 = DIRECTION ( 'NONE',  ( 0.000000000000000000, 0.000000000000000000, 1.000000000000000000 ) ) ;
#5207 = DIRECTION ( 'NONE',  ( 0.5000000000000051070, -0.8660254037844358210, 0.000000000000000000 ) ) ;
#5208 = DIRECTION ( 'NONE',  ( -1.000000000000000000, -0.000000000000000000, -0.000000000000000000 ) ) ;
#5209 = DIRECTION ( 'NONE',  ( 0.000000000000000000, -1.000000000000000000, 0.000000000000000000 ) ) ;
#5210 = VECTOR ( 'NONE', #5107, 1000.000000000000227 ) ;
#5211 = EDGE_CURVE ( 'NONE', #13758, #20315, #14966, .T. ) ;
#5212 = CARTESIAN_POINT ( 'NONE',  ( 56.06633208239072985, 77.22609791612467234, -8.065985790676100109 ) ) ;
#5213 = FACE_OUTER_BOUND ( 'NONE', #18739, .T. ) ;
#5214 = EDGE_LOOP ( 'NONE', ( #20219, #7705, #7820, #17180 ) ) ;
#5215 = SURFACE_SIDE_STYLE ('',( #5013 ) ) ;
#5216 = DIRECTION ( 'NONE',  ( -0.9987303135603810000, 0.000000000000000000, -0.05037619254750287656 ) ) ;
#5217 = DIRECTION ( 'NONE',  ( -1.000000000000000000, 0.000000000000000000, 0.000000000000000000 ) ) ;
#5218 = CARTESIAN_POINT ( 'NONE',  ( -11.87870293693008250, 79.99650906190652222, -12.16257741986773055 ) ) ;
#5219 = EDGE_CURVE ( 'NONE', #15362, #8267, #17812, .T. ) ;
#5220 = ORIENTED_EDGE ( 'NONE', *, *, #17144, .T. ) ;
#5221 = DIRECTION ( 'NONE',  ( 0.8660254037844370423, 0.5000000000000027756, 1.765692291717890446E-15 ) ) ;
#5222 = DIRECTION ( 'NONE',  ( 0.8660254037844371533, 0.5000000000000026645, 6.106226635438360972E-16 ) ) ;
#5223 = DIRECTION ( 'NONE',  ( 0.8660254037844370423, 0.5000000000000026645, -0.000000000000000000 ) ) ;
#5224 = ADVANCED_FACE ( 'NONE', ( #5276 ), #18225, .F. ) ;
#5225 = CARTESIAN_POINT ( 'NONE',  ( 82.23375342391803144, 58.06063708979128535, -24.22722688745409769 ) ) ;
#5226 = VECTOR ( 'NONE', #2617, 1000.000000000000000 ) ;
#5227 = CARTESIAN_POINT ( 'NONE',  ( -29.99999999999999645, 5.000000000000000888, 2.347807969642663029 ) ) ;
#5228 = CARTESIAN_POINT ( 'NONE',  ( 77.00490953756764156, 160.5799536996104280, 26.00000000000001066 ) ) ;
#5229 = ORIENTED_EDGE ( 'NONE', *, *, #1474, .F. ) ;
#5230 = CARTESIAN_POINT ( 'NONE',  ( 80.29132060388693048, 59.45028869689328133, -24.26604442088980917 ) ) ;
#5231 = CARTESIAN_POINT ( 'NONE',  ( 219.8702716421484809, 33.88892106552722794, -17.38313153181864479 ) ) ;
#5232 = EDGE_CURVE ( 'NONE', #18162, #11248, #16853, .T. ) ;
#5233 = EDGE_CURVE ( 'NONE', #19392, #16971, #16132, .T. ) ;
#5234 = VERTEX_POINT ( 'NONE', #13676 ) ;
#5235 = CARTESIAN_POINT ( 'NONE',  ( 201.8352900073124658, 26.48082042610822029, -14.39073202032135335 ) ) ;
#5236 = CARTESIAN_POINT ( 'NONE',  ( 1.499462569501769815, 53.04219685298476605, -3.436763594309801384 ) ) ;
#5237 = CARTESIAN_POINT ( 'NONE',  ( 1.399080956625346150, 76.99412170571200420, -3.489245206103287256 ) ) ;
#5238 = AXIS2_PLACEMENT_3D ( 'NONE', #9173, #10875, #10989 ) ;
#5239 = CARTESIAN_POINT ( 'NONE',  ( 208.3092871949524749, 11.56112132310348528, -12.02050488595160438 ) ) ;
#5240 = CARTESIAN_POINT ( 'NONE',  ( 216.3683575532813848, 33.19538101841231992, -14.00000000000004441 ) ) ;
#5241 = DIRECTION ( 'NONE',  ( -1.000000000000000000, -0.000000000000000000, -0.000000000000000000 ) ) ;
#5242 = AXIS2_PLACEMENT_3D ( 'NONE', #1706, #8155, #14667 ) ;
#5244 = ORIENTED_EDGE ( 'NONE', *, *, #13250, .F. ) ;
#5243 = ORIENTED_EDGE ( 'NONE', *, *, #2865, .T. ) ;
#5245 = ORIENTED_EDGE ( 'NONE', *, *, #13128, .F. ) ;
#5246 = CARTESIAN_POINT ( 'NONE',  ( 201.0525450381139194, 0.7212519096665224172, -23.06309126349794525 ) ) ;
#5247 = DIRECTION ( 'NONE',  ( 0.000000000000000000, 0.000000000000000000, 1.000000000000000000 ) ) ;
#5248 = EDGE_CURVE ( 'NONE', #10112, #17006, #4014, .T. ) ;
#5249 = VERTEX_POINT ( 'NONE', #7390 ) ;
#5250 = DIRECTION ( 'NONE',  ( 0.000000000000000000, 0.000000000000000000, -1.000000000000000000 ) ) ;
#5251 = LINE ( 'NONE', #8436, #20008 ) ;
#5252 = DIRECTION ( 'NONE',  ( 0.000000000000000000, 0.000000000000000000, 1.000000000000000000 ) ) ;
#5253 = ORIENTED_EDGE ( 'NONE', *, *, #16935, .F. ) ;
#5254 = DIRECTION ( 'NONE',  ( -0.6123724356957914727, -0.3535533905932749521, -0.7071067811865495711 ) ) ;
#5255 = CARTESIAN_POINT ( 'NONE',  ( 212.5077365114557040, 18.10909508356834863, -22.49869731917979365 ) ) ;
#5256 = TOROIDAL_SURFACE ( 'NONE', #16125, 0.9999999999999974465, 1.500000000000000000 ) ;
#5257 = ADVANCED_FACE ( 'NONE', ( #12302 ), #19644, .F. ) ;
#5258 = VERTEX_POINT ( 'NONE', #20026 ) ;
#5259 = VECTOR ( 'NONE', #10042, 1000.000000000000000 ) ;
#5260 = AXIS2_PLACEMENT_3D ( 'NONE', #13352, #18430, #15067 ) ;
#5261 = CARTESIAN_POINT ( 'NONE',  ( 215.9066831210195687, 15.94747990615854505, -12.62152863576173090 ) ) ;
#5262 = EDGE_CURVE ( 'NONE', #12427, #11581, #14847, .T. ) ;
#5263 = CARTESIAN_POINT ( 'NONE',  ( 209.8762589913677061, 12.46581291157636429, -13.00118852497347355 ) ) ;
#5264 = CARTESIAN_POINT ( 'NONE',  ( -33.23999054399477160, 55.56111691158302790, -0.8200133748984262949 ) ) ;
#5265 = CARTESIAN_POINT ( 'NONE',  ( -15.99999999999999289, 20.09941697557067997, 12.50000000000000000 ) ) ;
#5266 = CARTESIAN_POINT ( 'NONE',  ( 229.2667916872696310, 37.28720185707197743, -11.68692323064996685 ) ) ;
#5267 = ADVANCED_FACE ( 'NONE', ( #19912 ), #5692, .T. ) ;
#5268 = CARTESIAN_POINT ( 'NONE',  ( 220.2180084519553134, 35.41797800104779270, -14.00000000000005507 ) ) ;
#5270 = EDGE_LOOP ( 'NONE', ( #5198, #20606, #18436, #10211 ) ) ;
#5269 = ORIENTED_EDGE ( 'NONE', *, *, #9400, .F. ) ;
#5271 = AXIS2_PLACEMENT_3D ( 'NONE', #13947, #1321, #12356 ) ;
#5272 = ORIENTED_EDGE ( 'NONE', *, *, #15628, .F. ) ;
#5273 = CARTESIAN_POINT ( 'NONE',  ( 58.67095626531940411, 85.42695601701730368, -11.35807125314311072 ) ) ;
#5274 = ORIENTED_EDGE ( 'NONE', *, *, #1350, .T. ) ;
#5275 = VECTOR ( 'NONE', #15466, 1000.000000000000000 ) ;
#5276 = FACE_OUTER_BOUND ( 'NONE', #10013, .T. ) ;
#5277 = AXIS2_PLACEMENT_3D ( 'NONE', #5556, #3984, #16817 ) ;
#5278 = CARTESIAN_POINT ( 'NONE',  ( 212.9548847052525957, 4.941433797637768244, -14.00000000000005507 ) ) ;
#5279 = EDGE_LOOP ( 'NONE', ( #13045, #17684, #12503, #2516, #2214, #20077 ) ) ;
#5280 = CARTESIAN_POINT ( 'NONE',  ( 200.0157312721003393, 23.75418783301503112, -14.00000000000005507 ) ) ;
#5281 = CARTESIAN_POINT ( 'NONE',  ( 213.5545353545354601, 14.58946676000514486, -21.69368824361360382 ) ) ;
#5282 = VERTEX_POINT ( 'NONE', #18648 ) ;
#5283 = CARTESIAN_POINT ( 'NONE',  ( 191.8105349496822782, 16.77423392077770004, -4.915515517929134326 ) ) ;
#5284 = CARTESIAN_POINT ( 'NONE',  ( 184.9952905943350459, 3.535126980567751431, -22.00000000000009948 ) ) ;
#5285 = AXIS2_PLACEMENT_3D ( 'NONE', #4922, #5022, #11398 ) ;
#5286 = LINE ( 'NONE', #2136, #197 ) ;
#5287 = LINE ( 'NONE', #8693, #13640 ) ;
#5288 = ORIENTED_EDGE ( 'NONE', *, *, #20924, .T. ) ;
#5289 = LINE ( 'NONE', #14774, #16960 ) ;
#5290 = DIRECTION ( 'NONE',  ( -0.9367698044638387289, 0.000000000000000000, 0.3499461864984122483 ) ) ;
#5291 = FACE_OUTER_BOUND ( 'NONE', #12189, .T. ) ;
#5292 = ORIENTED_EDGE ( 'NONE', *, *, #833, .F. ) ;
#5293 = CARTESIAN_POINT ( 'NONE',  ( -15.99999999999999289, 80.00000000000000000, 0.000000000000000000 ) ) ;
#5294 = CARTESIAN_POINT ( 'NONE',  ( 201.9876756982950781, 25.95812089196162020, -12.80147382135962353 ) ) ;
#5295 = EDGE_CURVE ( 'NONE', #17359, #17685, #10465, .T. ) ;
#5296 = CARTESIAN_POINT ( 'NONE',  ( -11.68625644715183931, 65.74999999999995737, -2.528164662410434804 ) ) ;
#5297 = CARTESIAN_POINT ( 'NONE',  ( 77.91539758371193614, 51.99679936220445597, -12.14267250949680488 ) ) ;
#5299 = ORIENTED_EDGE ( 'NONE', *, *, #13692, .F. ) ;
#5298 = VERTEX_POINT ( 'NONE', #5378 ) ;
#5300 = AXIS2_PLACEMENT_3D ( 'NONE', #14742, #3672, #8128 ) ;
#5301 = VECTOR ( 'NONE', #2871, 1000.000000000000000 ) ;
#5302 = ORIENTED_EDGE ( 'NONE', *, *, #1024, .T. ) ;
#5303 = CARTESIAN_POINT ( 'NONE',  ( 226.5660535422584019, 42.29148661813671595, -16.31968669809488759 ) ) ;
#5304 = EDGE_LOOP ( 'NONE', ( #18606, #16668, #901, #18200 ) ) ;
#5305 = CARTESIAN_POINT ( 'NONE',  ( 75.40630481554458697, 52.49822515946223689, -16.08063866060412650 ) ) ;
#5306 = CARTESIAN_POINT ( 'NONE',  ( 198.4658173668363190, 5.877991368080599521, -5.291540431471293715 ) ) ;
#5307 = CARTESIAN_POINT ( 'NONE',  ( 218.0493302439821548, 9.761530332989567071, -8.625373497621339425 ) ) ;
#5308 = ORIENTED_EDGE ( 'NONE', *, *, #14148, .F. ) ;
#5309 = ADVANCED_FACE ( 'NONE', ( #11871, #18334, #2542 ), #947, .F. ) ;
#5310 = CARTESIAN_POINT ( 'NONE',  ( 218.2432760455571952, 38.19044168487747726, -15.10067325715080599 ) ) ;
#5311 = CARTESIAN_POINT ( 'NONE',  ( 226.0543776291551978, 42.52477616413780481, -11.99328011306285724 ) ) ;
#5312 = AXIS2_PLACEMENT_3D ( 'NONE', #10766, #9174, #19254 ) ;
#5313 = DIRECTION ( 'NONE',  ( -0.8660254037844360431, -0.5000000000000044409, 5.976026924694052093E-17 ) ) ;
#5314 = EDGE_LOOP ( 'NONE', ( #14238, #12408, #12374, #6867 ) ) ;
#5315 = CARTESIAN_POINT ( 'NONE',  ( 30.00000000000000000, 0.000000000000000000, 15.00000000000000000 ) ) ;
#5316 = EDGE_CURVE ( 'NONE', #5484, #20070, #15074, .T. ) ;
#5318 = CARTESIAN_POINT ( 'NONE',  ( 228.1971211027353377, 38.48692884174984385, -10.33191597617941504 ) ) ;
#5317 = VECTOR ( 'NONE', #2393, 1000.000000000000114 ) ;
#5319 = EDGE_CURVE ( 'NONE', #2221, #17006, #8508, .T. ) ;
#5320 = DIRECTION ( 'NONE',  ( 0.8660254037844372643, 0.5000000000000027756, -0.000000000000000000 ) ) ;
#5321 = CARTESIAN_POINT ( 'NONE',  ( -4.019148893687301438, 80.00000000016062529, -3.582299587995576573 ) ) ;
#5322 = ORIENTED_EDGE ( 'NONE', *, *, #2048, .F. ) ;
#5323 = DIRECTION ( 'NONE',  ( -0.000000000000000000, -1.000000000000000000, -0.000000000000000000 ) ) ;
#5324 = PLANE ( 'NONE',  #13946 ) ;
#5325 = CARTESIAN_POINT ( 'NONE',  ( -32.66093446721252747, 78.07057667199779871, -5.137872117311673925 ) ) ;
#5326 = CARTESIAN_POINT ( 'NONE',  ( 206.4681030732283205, 9.967063913005945963, -26.45271578590685380 ) ) ;
#5327=STYLED_ITEM('',(#20967),#17741);
#5328 = CARTESIAN_POINT ( 'NONE',  ( -27.93274434770766135, 6.474012523638976724, 3.820265228604878605 ) ) ;
#5329 = CARTESIAN_POINT ( 'NONE',  ( 5.000000000000004441, -4.685197434473809430, 6.071532165918824830E-15 ) ) ;
#5330 = ORIENTED_EDGE ( 'NONE', *, *, #16935, .T. ) ;
#5331 = AXIS2_PLACEMENT_3D ( 'NONE', #6055, #20693, #15738 ) ;
#5332 = PRODUCT_RELATED_PRODUCT_CATEGORY ( 'part', '', ( #18202 ) ) ;
#5333 = CARTESIAN_POINT ( 'NONE',  ( 82.31640018076895160, 62.45399354285202520, -25.25199697837627255 ) ) ;
#5334 = CARTESIAN_POINT ( 'NONE',  ( 219.3321254432009368, 36.95237238177238481, -10.52303454827236884 ) ) ;
#5335 = ORIENTED_EDGE ( 'NONE', *, *, #15580, .F. ) ;
#5336 = FACE_OUTER_BOUND ( 'NONE', #16621, .T. ) ;
#5337 = CARTESIAN_POINT ( 'NONE',  ( -4.511339306326391352, 60.05354679878421109, 4.930296734904765721 ) ) ;
#5338 = CARTESIAN_POINT ( 'NONE',  ( 212.9202825050182923, 6.800273240212296955, -24.96223045542567931 ) ) ;
#5339 = CARTESIAN_POINT ( 'NONE',  ( 195.8472345282168874, 4.366151861308305016, -18.11117897393217646 ) ) ;
#5340 = ADVANCED_FACE ( 'NONE', ( #13881 ), #5805, .F. ) ;
#5341 = DIRECTION ( 'NONE',  ( 0.5000000000000015543, -0.8660254037844377084, 0.000000000000000000 ) ) ;
#5342 = CARTESIAN_POINT ( 'NONE',  ( 208.1005406747554787, 4.017593997085510793, -27.13030671846408737 ) ) ;
#5343 = AXIS2_PLACEMENT_3D ( 'NONE', #19222, #20589, #19320 ) ;
#5344 = EDGE_CURVE ( 'NONE', #9197, #20000, #7192, .T. ) ;
#5346 = EDGE_LOOP ( 'NONE', ( #4293, #1161, #13965, #19682 ) ) ;
#5345 = VERTEX_POINT ( 'NONE', #20126 ) ;
#5347 = ORIENTED_EDGE ( 'NONE', *, *, #16416, .T. ) ;
#5348 = PLANE ( 'NONE',  #19659 ) ;
#5349 = DIRECTION ( 'NONE',  ( -0.5000000000000054401, 0.8660254037844354880, -0.000000000000000000 ) ) ;
#5350 = ORIENTED_EDGE ( 'NONE', *, *, #7794, .T. ) ;
#5351 = ORIENTED_EDGE ( 'NONE', *, *, #2161, .T. ) ;
#5352 = ORIENTED_EDGE ( 'NONE', *, *, #12394, .T. ) ;
#5353 = CARTESIAN_POINT ( 'NONE',  ( 81.03699745905494467, 60.80382008804202343, -0.1887428286780195308 ) ) ;
#5354 = CARTESIAN_POINT ( 'NONE',  ( 226.1656734413107870, 42.98496529531720256, -14.53826389233644356 ) ) ;
#5355 = CARTESIAN_POINT ( 'NONE',  ( 227.4555018439916125, 40.42444789286288653, -10.35599826740969398 ) ) ;
#5356 = ORIENTED_EDGE ( 'NONE', *, *, #5004, .F. ) ;
#5357 = EDGE_CURVE ( 'NONE', #16283, #4251, #13237, .T. ) ;
#5358 = DIRECTION ( 'NONE',  ( -0.3412765716093286716, 0.5911083614602702374, -0.7308359642781253607 ) ) ;
#5359 = CARTESIAN_POINT ( 'NONE',  ( 199.3787015603994917, 6.051018721616807206, -4.128377653168135986 ) ) ;
#5360 = EDGE_LOOP ( 'NONE', ( #10412, #4540, #5677, #18072 ) ) ;
#5361 = AXIS2_PLACEMENT_3D ( 'NONE', #18131, #10153, #13473 ) ;
#5362 = DIRECTION ( 'NONE',  ( -0.5000000000000049960, 0.8660254037844357100, -0.000000000000000000 ) ) ;
#5363 = EDGE_CURVE ( 'NONE', #5282, #5621, #5587, .T. ) ;
#5364 = CARTESIAN_POINT ( 'NONE',  ( 195.2174643819972744, 4.002553897860817500, -13.98704593443225797 ) ) ;
#5365 = FACE_OUTER_BOUND ( 'NONE', #2107, .T. ) ;
#5366 = CARTESIAN_POINT ( 'NONE',  ( -33.48120423251649669, 52.62637900463001728, -3.990501944831340353 ) ) ;
#5367 = CARTESIAN_POINT ( 'NONE',  ( -17.62170904672685978, 19.84043322078894889, 12.39812820015802686 ) ) ;
#5368 = VERTEX_POINT ( 'NONE', #13570 ) ;
#5369 = ADVANCED_FACE ( 'NONE', ( #16638 ), #15390, .T. ) ;
#5370 = DIRECTION ( 'NONE',  ( 1.000000000000000000, 0.000000000000000000, -0.000000000000000000 ) ) ;
#5371 = LINE ( 'NONE', #18327, #15472 ) ;
#5373 = ORIENTED_EDGE ( 'NONE', *, *, #19650, .T. ) ;
#5372 = VERTEX_POINT ( 'NONE', #13781 ) ;
#5374 = CARTESIAN_POINT ( 'NONE',  ( 62.89558499432746430, 78.00608458378800947, -12.44082293186782628 ) ) ;
#5375 = VERTEX_POINT ( 'NONE', #20227 ) ;
#5376 = AXIS2_PLACEMENT_3D ( 'NONE', #7590, #13868, #13661 ) ;
#5377 = ORIENTED_EDGE ( 'NONE', *, *, #16011, .F. ) ;
#5378 = CARTESIAN_POINT ( 'NONE',  ( 199.0852767235472527, -1.187371071960172664, -9.928836400542227381 ) ) ;
#5379 = CYLINDRICAL_SURFACE ( 'NONE', #15123, 5.000000000000000888 ) ;
#5380 = EDGE_CURVE ( 'NONE', #2174, #2247, #14597, .T. ) ;
#5381 = EDGE_CURVE ( 'NONE', #18033, #13343, #6010, .T. ) ;
#5382 = VERTEX_POINT ( 'NONE', #18862 ) ;
#5383 = CARTESIAN_POINT ( 'NONE',  ( 205.6089461623839441, 14.12607661844890039, -25.65046807331635748 ) ) ;
#5384 = AXIS2_PLACEMENT_3D ( 'NONE', #5772, #12758, #9340 ) ;
#5385 = CARTESIAN_POINT ( 'NONE',  ( 208.8107687779841228, 4.427644383670616079, -14.00000000000005507 ) ) ;
#5386 = EDGE_LOOP ( 'NONE', ( #4445, #6766, #20389, #17477, #13265 ) ) ;
#5387 =( REPRESENTATION_RELATIONSHIP ('NONE','NONE', #4634, #8398 ) REPRESENTATION_RELATIONSHIP_WITH_TRANSFORMATION ( #17819 )SHAPE_REPRESENTATION_RELATIONSHIP( ) );
#5388 = DIRECTION ( 'NONE',  ( 0.8660254037844362651, 0.5000000000000043299, 0.000000000000000000 ) ) ;
#5389 = DIRECTION ( 'NONE',  ( 0.000000000000000000, 0.000000000000000000, 1.000000000000000000 ) ) ;
#5390 = EDGE_CURVE ( 'NONE', #12589, #10573, #1683, .T. ) ;
#5391 = DIRECTION ( 'NONE',  ( -0.000000000000000000, -0.000000000000000000, 1.000000000000000000 ) ) ;
#5392 = FACE_OUTER_BOUND ( 'NONE', #20518, .T. ) ;
#5393 = DIRECTION ( 'NONE',  ( 0.000000000000000000, 0.000000000000000000, -1.000000000000000000 ) ) ;
#5394 = CARTESIAN_POINT ( 'NONE',  ( -28.94340094228533644, 73.00589460461614522, 0.1996236911382455459 ) ) ;
#5395 = AXIS2_PLACEMENT_3D ( 'NONE', #16816, #3767, #2294 ) ;
#5396 = CARTESIAN_POINT ( 'NONE',  ( 199.2144802262915846, 21.04890371929339921, -14.00000000000005507 ) ) ;
#5397 = LINE ( 'NONE', #13483, #10884 ) ;
#5398 = EDGE_LOOP ( 'NONE', ( #8930, #7080, #9377, #3699, #11160, #7577, #10577, #16346, #8651 ) ) ;
#5399 = EDGE_CURVE ( 'NONE', #5150, #835, #7504, .T. ) ;
#5400 = CARTESIAN_POINT ( 'NONE',  ( 80.95969170222095102, 60.64095424398406919, -0.2422237528172087040 ) ) ;
#5401 = DIRECTION ( 'NONE',  ( 0.8660254037844355990, 0.5000000000000054401, 0.000000000000000000 ) ) ;
#5402 = CARTESIAN_POINT ( 'NONE',  ( 80.55381169140011366, 52.82318510880671170, -4.391639923843643878 ) ) ;
#5404 = ORIENTED_EDGE ( 'NONE', *, *, #3422, .F. ) ;
#5403 = ORIENTED_EDGE ( 'NONE', *, *, #10799, .T. ) ;
#5405 = VECTOR ( 'NONE', #4163, 1000.000000000000114 ) ;
#5406 = CARTESIAN_POINT ( 'NONE',  ( 0.000000000000000000, 0.000000000000000000, 0.000000000000000000 ) ) ;
#5407=STYLED_ITEM('',(#20988),#3811);
#5408 = VECTOR ( 'NONE', #17869, 1000.000000000000000 ) ;
#5409 = DIRECTION ( 'NONE',  ( 0.000000000000000000, -1.000000000000000000, 0.000000000000000000 ) ) ;
#5410 = ORIENTED_EDGE ( 'NONE', *, *, #6587, .F. ) ;
#5411 = CARTESIAN_POINT ( 'NONE',  ( 75.89995346768556317, 53.15581343745467535, -7.100154262375115266 ) ) ;
#5412 = CARTESIAN_POINT ( 'NONE',  ( -20.08622074598449458, 79.99311222855624237, -11.99929078098927526 ) ) ;
#5413 = DIRECTION ( 'NONE',  ( -1.000000000000000000, 0.000000000000000000, 0.000000000000000000 ) ) ;
#5414 = CARTESIAN_POINT ( 'NONE',  ( 196.1661066256804986, 4.019203490823548997, -8.415281845791808379 ) ) ;
#5415 = VECTOR ( 'NONE', #4335, 1000.000000000000227 ) ;
#5416 = DIRECTION ( 'NONE',  ( 0.8660254037844344888, 0.5000000000000069944, 0.000000000000000000 ) ) ;
#5417 =( BOUNDED_SURFACE ( )  B_SPLINE_SURFACE ( 3, 2, ( 
 ( #18855, #19167, #4226 ),
 ( #17261, #20534, #14098 ),
 ( #1160, #20746, #9393 ),
 ( #10673, #2746, #17373 ),
 ( #9188, #15694, #6006 ),
 ( #12496, #7710, #18955 ),
 ( #14207, #20636, #6109 ),
 ( #12605, #19067, #11007 ),
 ( #15890, #12918, #8011 ),
 ( #13404, #11707, #19753 ),
 ( #477, #575, #18173 ),
 ( #5321, #11922, #16692 ),
 ( #12814, #10197, #11215 ),
 ( #17689, #15120, #2170 ),
 ( #8621, #16102, #1673 ),
 ( #14522, #16002, #19933 ),
 ( #3741, #7912, #8113 ),
 ( #14628, #7025, #373 ),
 ( #18385, #14412, #6818 ),
 ( #20841, #17784, #3638 ),
 ( #8519, #9707, #5424 ),
 ( #3156, #9606, #10089 ),
 ( #15018, #19853, #13512 ),
 ( #6418, #19958, #11810 ),
 ( #1465, #3252, #9501 ),
 ( #19271, #1568, #5218 ),
 ( #6317, #11318, #19371 ),
 ( #16579, #18272, #16199 ),
 ( #13304, #4844, #6919 ),
 ( #4740, #2064, #12025 ),
 ( #20383, #2270, #15641 ),
 ( #890, #788, #8935 ),
 ( #20174, #10517, #10731 ),
 ( #20073, #1108, #17211 ) ),
 .UNSPECIFIED., .F., .F., .T. ) 
 B_SPLINE_SURFACE_WITH_KNOTS ( ( 4, 2, 2, 2, 2, 2, 2, 2, 2, 2, 2, 2, 2, 2, 2, 2, 4 ),
 ( 3, 3 ),
 ( 0.01278509310405297195, 0.01434830319407976937, 0.01591151328410656679, 0.01669311832911996724, 0.01747472337413336421, 0.01903793346416016163, 0.02060114355418695906, 0.02216435364421375648, 0.02529077382426735479, 0.02685398391429415221, 0.02841719400432095310, 0.03154361418437454795, 0.03310682427440134190, 0.03467003436442814279, 0.03623324445445494368, 0.03701484949946834413, 0.03779645454448173764 ),
 ( 0.000000000000000000, 1.000000000000000000 ),
 .UNSPECIFIED. ) 
 GEOMETRIC_REPRESENTATION_ITEM ( )  RATIONAL_B_SPLINE_SURFACE ( (
 ( 1.000000000000000000, 0.7167790485004654766, 1.000000000000000000),
 ( 1.000000000000000000, 0.7293845257054283326, 1.000000000000000000),
 ( 1.000000000000000000, 0.7423068803280219452, 1.000000000000000000),
 ( 1.000000000000000000, 0.7686138469777443749, 1.000000000000000000),
 ( 1.000000000000000000, 0.7816781719487659874, 1.000000000000000000),
 ( 1.000000000000000000, 0.8009424076555987648, 1.000000000000000000),
 ( 1.000000000000000000, 0.8073105603346681924, 1.000000000000000000),
 ( 1.000000000000000000, 0.8199112611633488923, 1.000000000000000000),
 ( 1.000000000000000000, 0.8261570471473095312, 1.000000000000000000),
 ( 1.000000000000000000, 0.8443914605100146797, 1.000000000000000000),
 ( 1.000000000000000000, 0.8559617003904390620, 1.000000000000000000),
 ( 1.000000000000000000, 0.8778584927322264919, 1.000000000000000000),
 ( 1.000000000000000000, 0.8881844774554628064, 1.000000000000000000),
 ( 1.000000000000000000, 0.9075144288648415714, 1.000000000000000000),
 ( 1.000000000000000000, 0.9165151951639417538, 1.000000000000000000),
 ( 1.000000000000000000, 0.9409273377065782151, 1.000000000000000000),
 ( 1.000000000000000000, 0.9539926103733148421, 1.000000000000000000),
 ( 1.000000000000000000, 0.9694264545132288413, 1.000000000000000000),
 ( 1.000000000000000000, 0.9738877056526868969, 1.000000000000000000),
 ( 1.000000000000000000, 0.9815112523103146636, 1.000000000000000000),
 ( 1.000000000000000000, 0.9846522094487469845, 1.000000000000000000),
 ( 1.000000000000000000, 0.9924326897349095011, 1.000000000000000000),
 ( 1.000000000000000000, 0.9954310229819317568, 1.000000000000000000),
 ( 1.000000000000000000, 0.9981072485120819904, 1.000000000000000000),
 ( 1.000000000000000000, 0.9986952519232751291, 1.000000000000000000),
 ( 1.000000000000000000, 0.9994860253291516505, 1.000000000000000000),
 ( 1.000000000000000000, 0.9996937099786900038, 1.000000000000000000),
 ( 1.000000000000000000, 0.9999366964164366767, 1.000000000000000000),
 ( 1.000000000000000000, 0.9999724247964512092, 1.000000000000000000),
 ( 1.000000000000000000, 0.9999959980224297773, 1.000000000000000000),
 ( 1.000000000000000000, 0.9999982534776523657, 1.000000000000000000),
 ( 1.000000000000000000, 1.000000247701407607, 1.000000000000000000),
 ( 1.000000000000000000, 1.000000000000000000, 1.000000000000000000),
 ( 1.000000000000000000, 1.000000000000000000, 1.000000000000000000) ) ) 
 REPRESENTATION_ITEM ( '' )  SURFACE ( )  );
#5418 = DIRECTION ( 'NONE',  ( 0.8426815769442655979, 0.4865224352899170102, -0.2306158707424410814 ) ) ;
#5419 = CARTESIAN_POINT ( 'NONE',  ( 199.3161926515599589, -0.7964524749548287375, -19.43577154980779298 ) ) ;
#5420 = ORIENTED_EDGE ( 'NONE', *, *, #14113, .T. ) ;
#5421 = AXIS2_PLACEMENT_3D ( 'NONE', #16406, #12812, #8329 ) ;
#5422 = CARTESIAN_POINT ( 'NONE',  ( 197.6529114527598381, 5.408659919762685675, -6.286464976498783663 ) ) ;
#5423 = CARTESIAN_POINT ( 'NONE',  ( 196.3164214246273218, 4.637037042251114904, -19.36714384557513924 ) ) ;
#5424 = CARTESIAN_POINT ( 'NONE',  ( -6.567413104170348070, 79.88387937455904364, -10.62823034224189556 ) ) ;
#5426 = ORIENTED_EDGE ( 'NONE', *, *, #14613, .F. ) ;
#5425 = ORIENTED_EDGE ( 'NONE', *, *, #5666, .T. ) ;
#5427 = ORIENTED_EDGE ( 'NONE', *, *, #19181, .F. ) ;
#5428 = CARTESIAN_POINT ( 'NONE',  ( 64.99529059433392320, 211.3812238888322952, 6.000000000000009770 ) ) ;
#5429 = CARTESIAN_POINT ( 'NONE',  ( 222.1691453665456493, 32.03850973245414480, -13.97349461567483964 ) ) ;
#5430 = DIRECTION ( 'NONE',  ( -0.8660254037844380415, -0.5000000000000014433, -0.000000000000000000 ) ) ;
#5431 = CARTESIAN_POINT ( 'NONE',  ( 80.94022347753882229, 67.15523189662422965, -25.58958341134216852 ) ) ;
#5432 = CARTESIAN_POINT ( 'NONE',  ( -29.99999999999999645, 5.000000000000000000, 10.11936314359214606 ) ) ;
#5433 =( LENGTH_UNIT ( ) NAMED_UNIT ( * ) SI_UNIT ( .MILLI., .METRE. ) );
#5434 = DIRECTION ( 'NONE',  ( 0.000000000000000000, -0.4999999999999987232, 0.8660254037844393737 ) ) ;
#5435 = VERTEX_POINT ( 'NONE', #20640 ) ;
#5436 = CONICAL_SURFACE ( 'NONE', #11902, 10.85470691220533190, 0.8171114040043576665 ) ;
#5437 = EDGE_CURVE ( 'NONE', #6217, #5656, #20752, .T. ) ;
#5438 = CARTESIAN_POINT ( 'NONE',  ( 81.73869807597520776, 63.32742336881895540, -25.39460242813820656 ) ) ;
#5439 = CARTESIAN_POINT ( 'NONE',  ( 61.44066546377918314, 83.29626644201148622, -18.49058275380094685 ) ) ;
#5440 = ORIENTED_EDGE ( 'NONE', *, *, #18506, .T. ) ;
#5441 = CARTESIAN_POINT ( 'NONE',  ( 201.9048576179487213, 26.22121821873378877, -14.91588034066295521 ) ) ;
#5442 = CARTESIAN_POINT ( 'NONE',  ( 0.4495246258101979753, 59.24330822791731777, 1.356054076072180425 ) ) ;
#5443 = FACE_BOUND ( 'NONE', #20780, .T. ) ;
#5444 = CARTESIAN_POINT ( 'NONE',  ( 205.0662616026534693, 10.91332106064940888, -14.00000000000005507 ) ) ;
#5445 = CARTESIAN_POINT ( 'NONE',  ( 97.26699134085764342, 198.9478798014807808, 9.463061291710214817 ) ) ;
#5446 = CARTESIAN_POINT ( 'NONE',  ( 61.15142905248526262, 218.0389873765740845, 45.89527237623694589 ) ) ;
#5448 = ORIENTED_EDGE ( 'NONE', *, *, #18902, .T. ) ;
#5447 = ORIENTED_EDGE ( 'NONE', *, *, #13396, .T. ) ;
#5449 = B_SPLINE_CURVE_WITH_KNOTS ( 'NONE', 3,
 ( #8037, #11549, #3592, #18122 ),
 .UNSPECIFIED., .F., .F.,
 ( 4, 4 ),
 ( 0.0001020613991901207350, 0.0009560471371670607125 ),
 .UNSPECIFIED. ) ;
#5450 = ORIENTED_EDGE ( 'NONE', *, *, #4034, .T. ) ;
#5451 = ORIENTED_EDGE ( 'NONE', *, *, #2952, .T. ) ;
#5452 = DIRECTION ( 'NONE',  ( -0.000000000000000000, -0.000000000000000000, -1.000000000000000000 ) ) ;
#5454 = DIRECTION ( 'NONE',  ( 0.5000000000000043299, -0.8660254037844361541, -1.214306433183764966E-16 ) ) ;
#5453 = AXIS2_PLACEMENT_3D ( 'NONE', #13516, #20078, #3745 ) ;
#5455 = ADVANCED_FACE ( 'NONE', ( #15588 ), #15286, .T. ) ;
#5456 = VECTOR ( 'NONE', #15711, 1000.000000000000000 ) ;
#5457 = VERTEX_POINT ( 'NONE', #10786 ) ;
#5458 = CARTESIAN_POINT ( 'NONE',  ( 81.06711713768373784, 65.00000000000000000, 0.4999999999999962252 ) ) ;
#5459 = DIRECTION ( 'NONE',  ( 0.3412765716093336121, -0.5911083614602787861, -0.7308359642781161458 ) ) ;
#5460 = DIRECTION ( 'NONE',  ( 0.8660254037844358210, 0.5000000000000046629, 0.000000000000000000 ) ) ;
#5461 = ORIENTED_EDGE ( 'NONE', *, *, #16804, .F. ) ;
#5462 = AXIS2_PLACEMENT_3D ( 'NONE', #2162, #8615, #7123 ) ;
#5463 = CARTESIAN_POINT ( 'NONE',  ( -14.99999999999999645, 0.000000000000000000, 15.00000000000000000 ) ) ;
#5464 = CARTESIAN_POINT ( 'NONE',  ( 209.0038672028605049, 11.96213727764292756, -16.47016555539322269 ) ) ;
#5465 = EDGE_CURVE ( 'NONE', #19461, #15690, #666, .T. ) ;
#5466 = ORIENTED_EDGE ( 'NONE', *, *, #13945, .T. ) ;
#5467 = CIRCLE ( 'NONE', #10903, 4.057500000000000107 ) ;
#5468 = ADVANCED_FACE ( 'NONE', ( #2751 ), #17289, .F. ) ;
#5469 = AXIS2_PLACEMENT_3D ( 'NONE', #18456, #13695, #20145 ) ;
#5470 = DIRECTION ( 'NONE',  ( -0.8660254037844361541, -0.5000000000000045519, 5.976026924694053325E-17 ) ) ;
#5471 = AXIS2_PLACEMENT_3D ( 'NONE', #6807, #14899, #567 ) ;
#5472 = AXIS2_PLACEMENT_3D ( 'NONE', #14302, #12697, #19155 ) ;
#5473 = DIRECTION ( 'NONE',  ( 0.9573016540814832664, -0.2890908907123435068, 8.927808436751186653E-17 ) ) ;
#5474 = CARTESIAN_POINT ( 'NONE',  ( -28.01889434176855431, 52.37691837744655743, -4.370015612845434383 ) ) ;
#5475 = CARTESIAN_POINT ( 'NONE',  ( 207.0496559082687043, 3.410865394267065032, -2.341985411376944271 ) ) ;
#5476 = ORIENTED_EDGE ( 'NONE', *, *, #19219, .T. ) ;
#5477 = CARTESIAN_POINT ( 'NONE',  ( 32.39721438298033007, 261.8427481158985302, -22.00000000000000355 ) ) ;
#5478 = LINE ( 'NONE', #14957, #17133 ) ;
#5479 = ADVANCED_FACE ( 'NONE', ( #17480 ), #12404, .F. ) ;
#5481 = ORIENTED_EDGE ( 'NONE', *, *, #9926, .F. ) ;
#5480 = ORIENTED_EDGE ( 'NONE', *, *, #12208, .T. ) ;
#5482 = CARTESIAN_POINT ( 'NONE',  ( 58.60004645507417820, 85.48142452582160900, -11.88094507543154421 ) ) ;
#5483 = ORIENTED_EDGE ( 'NONE', *, *, #19229, .T. ) ;
#5484 = VERTEX_POINT ( 'NONE', #9192 ) ;
#5485 = VERTEX_POINT ( 'NONE', #7817 ) ;
#5486 = DIRECTION ( 'NONE',  ( 0.8660254037844370423, 0.5000000000000026645, -0.000000000000000000 ) ) ;
#5487 = CARTESIAN_POINT ( 'NONE',  ( 34.99529059433364608, 263.3427481158985302, 1.000000000000028644 ) ) ;
#5488 = CIRCLE ( 'NONE', #10218, 4.389613146203297234 ) ;
#5489 = EDGE_CURVE ( 'NONE', #772, #18586, #1164, .T. ) ;
#5490 = VECTOR ( 'NONE', #19348, 1000.000000000000000 ) ;
#5491 = ORIENTED_EDGE ( 'NONE', *, *, #16783, .F. ) ;
#5492 = DIRECTION ( 'NONE',  ( 0.4272097022732466165, -0.7399489098236303741, 0.5195839500354345608 ) ) ;
#5493 = CIRCLE ( 'NONE', #2875, 14.99999999999999645 ) ;
#5494 = EDGE_CURVE ( 'NONE', #6871, #9039, #14317, .T. ) ;
#5495 = CARTESIAN_POINT ( 'NONE',  ( 205.8264633344831225, 9.596613037118636669, -14.00000000000005507 ) ) ;
#5496 = CARTESIAN_POINT ( 'NONE',  ( 220.4648716527350132, 34.34252521936895874, -10.59705062504283646 ) ) ;
#5497 = PRODUCT_DEFINITION_SHAPE ( 'NONE', 'NONE',  #20951 ) ;
#5498 = CARTESIAN_POINT ( 'NONE',  ( 219.9164680944309396, 33.80890646304445113, -10.64970491435236255 ) ) ;
#5499 = CARTESIAN_POINT ( 'NONE',  ( -15.99999999999999289, 15.09941697557068530, 0.9999999999999991118 ) ) ;
#5500 = DIRECTION ( 'NONE',  ( -0.5000000000000043299, 0.8660254037844360431, 0.000000000000000000 ) ) ;
#5501 = CARTESIAN_POINT ( 'NONE',  ( 205.0662616026534693, 10.91332106064940888, -14.00000000000005507 ) ) ;
#5502 = AXIS2_PLACEMENT_3D ( 'NONE', #5060, #8348, #13559 ) ;
#5503 = ADVANCED_FACE ( 'NONE', ( #7612 ), #20539, .T. ) ;
#5504 = ORIENTED_EDGE ( 'NONE', *, *, #2268, .F. ) ;
#5505 = CARTESIAN_POINT ( 'NONE',  ( 4.000000000000000000, -3.755786496842899057E-15, -3.047499999999999876 ) ) ;
#5506 = DIRECTION ( 'NONE',  ( -0.5000000000000054401, 0.8660254037844354880, -0.000000000000000000 ) ) ;
#5507 = CARTESIAN_POINT ( 'NONE',  ( 215.9066831210195687, 15.94747990615854505, -12.62152863576173090 ) ) ;
#5508 = EDGE_CURVE ( 'NONE', #12009, #7423, #19172, .T. ) ;
#5509 = ORIENTED_EDGE ( 'NONE', *, *, #8242, .T. ) ;
#5510 = CARTESIAN_POINT ( 'NONE',  ( -3.049535234737931866, 65.74999999999998579, 3.381771649840966010 ) ) ;
#5511 = ORIENTED_EDGE ( 'NONE', *, *, #6157, .T. ) ;
#5512 = CARTESIAN_POINT ( 'NONE',  ( -29.99999999999999645, 5.000000000000000000, 15.00000000000000000 ) ) ;
#5513 = DIRECTION ( 'NONE',  ( 0.8660254037844352659, 0.5000000000000056621, 0.000000000000000000 ) ) ;
#5514 = EDGE_CURVE ( 'NONE', #19519, #504, #17377, .T. ) ;
#5515 = ORIENTED_EDGE ( 'NONE', *, *, #5834, .F. ) ;
#5516 = B_SPLINE_CURVE_WITH_KNOTS ( 'NONE', 3,
 ( #7330, #8927, #17307, #9231 ),
 .UNSPECIFIED., .F., .F.,
 ( 4, 4 ),
 ( 4.013058786123878417E-07, 0.0004524545476584834248 ),
 .UNSPECIFIED. ) ;
#5517 = ADVANCED_BREP_SHAPE_REPRESENTATION ( '', ( #10635, #18233 ), #2676 ) ;
#5518 = CARTESIAN_POINT ( 'NONE',  ( -15.99999999999998934, 91.51038572010834571, 1.402686560653121361E-15 ) ) ;
#5519 = CIRCLE ( 'NONE', #14698, 4.389613146203297234 ) ;
#5520 = LINE ( 'NONE', #18154, #555 ) ;
#5521 = VERTEX_POINT ( 'NONE', #3054 ) ;
#5522 = CARTESIAN_POINT ( 'NONE',  ( 81.70617321326079718, 62.71419586981366479, -25.30228666757756528 ) ) ;
#5523 = EDGE_CURVE ( 'NONE', #10176, #9778, #4318, .T. ) ;
#5524 = CARTESIAN_POINT ( 'NONE',  ( -25.43258689582962973, 79.88387937455904364, -10.62823034224189911 ) ) ;
#5525 = CARTESIAN_POINT ( 'NONE',  ( 211.7650478275019168, 6.133298188171013798, -25.44774858730800560 ) ) ;
#5526 = CARTESIAN_POINT ( 'NONE',  ( 219.1556129512320013, 10.40024295182009517, -13.98474561060134747 ) ) ;
#5527 = VERTEX_POINT ( 'NONE', #12820 ) ;
#5528 = CARTESIAN_POINT ( 'NONE',  ( 182.3972143829817867, 2.035126980567763866, -22.00000000000009948 ) ) ;
#5529 = EDGE_CURVE ( 'NONE', #12589, #9246, #6114, .T. ) ;
#5530 = DIRECTION ( 'NONE',  ( -0.5000000000000054401, 0.8660254037844354880, -0.000000000000000000 ) ) ;
#5531 = DIRECTION ( 'NONE',  ( -0.5000000000000049960, 0.8660254037844357100, -0.000000000000000000 ) ) ;
#5532 = ORIENTED_EDGE ( 'NONE', *, *, #11081, .F. ) ;
#5533 = VECTOR ( 'NONE', #8257, 1000.000000000000227 ) ;
#5534 = VECTOR ( 'NONE', #9628, 1000.000000000000114 ) ;
#5535 = CARTESIAN_POINT ( 'NONE',  ( 87.00490953756771262, 143.2594456239216925, 1.000000000000007772 ) ) ;
#5536 = DIRECTION ( 'NONE',  ( 0.000000000000000000, 0.000000000000000000, -1.000000000000000000 ) ) ;
#5537 = DIRECTION ( 'NONE',  ( -0.5000000000000008882, 0.8660254037844381525, 0.000000000000000000 ) ) ;
#5538 = PLANE ( 'NONE',  #16869 ) ;
#5540 = ORIENTED_EDGE ( 'NONE', *, *, #10434, .F. ) ;
#5539 = ORIENTED_EDGE ( 'NONE', *, *, #5023, .F. ) ;
#5541 = ORIENTED_EDGE ( 'NONE', *, *, #5679, .F. ) ;
#5542 = CARTESIAN_POINT ( 'NONE',  ( 228.8726778135066127, 37.31683029529983742, -16.83383072344321008 ) ) ;
#5543 = DIRECTION ( 'NONE',  ( 0.8660254037844361541, 0.5000000000000044409, -5.976026924694052093E-17 ) ) ;
#5544 = LINE ( 'NONE', #12134, #18526 ) ;
#5545 = CARTESIAN_POINT ( 'NONE',  ( 78.90035330931522140, 69.25335659932615329, -25.39095082874599285 ) ) ;
#5546 = AXIS2_PLACEMENT_3D ( 'NONE', #17980, #3546, #10913 ) ;
#5547 = LINE ( 'NONE', #8531, #20134 ) ;
#5548 = ORIENTED_EDGE ( 'NONE', *, *, #7269, .F. ) ;
#5549 = CARTESIAN_POINT ( 'NONE',  ( 81.75619180876375935, 56.44393855648663560, -23.41859921127574395 ) ) ;
#5550 = CARTESIAN_POINT ( 'NONE',  ( 58.81500316096885683, 85.31629705828423482, -14.27754138227609104 ) ) ;
#5551 = EDGE_LOOP ( 'NONE', ( #2149, #11995, #3511, #13734, #2622 ) ) ;
#5552 = CARTESIAN_POINT ( 'NONE',  ( 201.8258405466010572, 26.51993739047028242, -14.19778417152125805 ) ) ;
#5553 = CARTESIAN_POINT ( 'NONE',  ( 30.10683012259193703, 5.000000000000000000, 0.000000000000000000 ) ) ;
#5554 = CARTESIAN_POINT ( 'NONE',  ( -35.00000000000000000, 64.25000000000000000, 1.479896280015796650 ) ) ;
#5555 = DIRECTION ( 'NONE',  ( 0.000000000000000000, 0.000000000000000000, -1.000000000000000000 ) ) ;
#5556 = CARTESIAN_POINT ( 'NONE',  ( 37.85427444295662269, 178.3908428320656299, 11.00000000000001243 ) ) ;
#5558 = ORIENTED_EDGE ( 'NONE', *, *, #11432, .F. ) ;
#5557 = ORIENTED_EDGE ( 'NONE', *, *, #15750, .T. ) ;
#5559 = EDGE_LOOP ( 'NONE', ( #4035, #20098, #11327, #17750, #6700 ) ) ;
#5560 = CIRCLE ( 'NONE', #13713, 13.50000000000000711 ) ;
#5561 = CARTESIAN_POINT ( 'NONE',  ( 202.6438527999323185, 0.8671737836725290638, -4.409371045252821197 ) ) ;
#5562 = CARTESIAN_POINT ( 'NONE',  ( 229.2419223966291497, 37.33027673200943042, -16.37421369872756571 ) ) ;
#5563 = ORIENTED_EDGE ( 'NONE', *, *, #4857, .T. ) ;
#5564 = EDGE_CURVE ( 'NONE', #2098, #5258, #8016, .T. ) ;
#5565 = CARTESIAN_POINT ( 'NONE',  ( 78.90361596372913766, 57.31366504278730645, -2.008240199223393141 ) ) ;
#5566 = DIRECTION ( 'NONE',  ( -0.8660254037844360431, -0.5000000000000045519, 7.398944170774818708E-15 ) ) ;
#5567 = DIRECTION ( 'NONE',  ( 0.5000000000000054401, -0.8660254037844354880, 0.000000000000000000 ) ) ;
#5568 = ORIENTED_EDGE ( 'NONE', *, *, #8290, .F. ) ;
#5569 = ORIENTED_EDGE ( 'NONE', *, *, #17776, .T. ) ;
#5570 = CARTESIAN_POINT ( 'NONE',  ( 220.2180084519553134, 35.41797800104779270, -14.00000000000005507 ) ) ;
#5571 = ORIENTED_EDGE ( 'NONE', *, *, #19483, .T. ) ;
#5572 = CLOSED_SHELL ( 'NONE', ( #7412, #6367, #18355, #20032, #19598, #9344, #4164, #8946, #7534, #18464, #8305, #12657, #5703, #15409, #20562, #8356, #3960, #9417, #10656, #6638, #6227, #12614, #848, #20649, #14235 ) ) ;
#5573 = LINE ( 'NONE', #9176, #7764 ) ;
#5574 = EDGE_CURVE ( 'NONE', #1000, #13448, #11524, .T. ) ;
#5575 = VECTOR ( 'NONE', #12538, 1000.000000000000227 ) ;
#5576 = FACE_OUTER_BOUND ( 'NONE', #13860, .T. ) ;
#5577 = CARTESIAN_POINT ( 'NONE',  ( -24.74148270909007152, 49.98498879254805161, -8.950542976129836958 ) ) ;
#5578 = CARTESIAN_POINT ( 'NONE',  ( 209.4254563108873413, 4.782534396259798370, -2.075899210536075401 ) ) ;
#5579 = ORIENTED_EDGE ( 'NONE', *, *, #11192, .F. ) ;
#5580 = PLANE ( 'NONE',  #4549 ) ;
#5581 = CARTESIAN_POINT ( 'NONE',  ( -27.90532276960012936, 55.94151689669796923, 3.821265830397637231 ) ) ;
#5583 = ORIENTED_EDGE ( 'NONE', *, *, #18469, .T. ) ;
#5582 = ORIENTED_EDGE ( 'NONE', *, *, #20624, .T. ) ;
#5584 = CARTESIAN_POINT ( 'NONE',  ( 57.60739473171254588, 76.56951856390271871, -18.44378120684195110 ) ) ;
#5585 = EDGE_CURVE ( 'NONE', #10070, #10118, #19464, .T. ) ;
#5586 = EDGE_CURVE ( 'NONE', #17970, #2546, #19309, .T. ) ;
#5587 = LINE ( 'NONE', #7088, #3729 ) ;
#5588 = VECTOR ( 'NONE', #17356, 1000.000000000000227 ) ;
#5589 = FACE_OUTER_BOUND ( 'NONE', #18000, .T. ) ;
#5590 = VERTEX_POINT ( 'NONE', #19678 ) ;
#5591 = VECTOR ( 'NONE', #10582, 999.9999999999998863 ) ;
#5592 = ORIENTED_EDGE ( 'NONE', *, *, #15285, .T. ) ;
#5593 = LINE ( 'NONE', #7296, #10729 ) ;
#5594 = AXIS2_PLACEMENT_3D ( 'NONE', #1816, #7858, #11458 ) ;
#5595 = B_SPLINE_CURVE_WITH_KNOTS ( 'NONE', 3,
 ( #7044, #2289, #7151, #4298 ),
 .UNSPECIFIED., .F., .F.,
 ( 4, 4 ),
 ( 0.000000000000000000, 0.001416029653785004505 ),
 .UNSPECIFIED. ) ;
#5596 = CARTESIAN_POINT ( 'NONE',  ( 220.9606893667113638, 33.51376855353427686, -16.94731950718130520 ) ) ;
#5597 = DIRECTION ( 'NONE',  ( 1.000000000000000000, -0.000000000000000000, -0.000000000000000000 ) ) ;
#5598 = CARTESIAN_POINT ( 'NONE',  ( -14.69197289804462159, 19.93670296710511636, 12.43566393466945108 ) ) ;
#5599 = PRODUCT_DEFINITION ( 'UNKNOWN', '', #16555, #10631 ) ;
#5600 = EDGE_LOOP ( 'NONE', ( #11772, #10645, #11553, #20799, #12144, #9733 ) ) ;
#5601 = CARTESIAN_POINT ( 'NONE',  ( 211.7650478275019168, 6.133298188171013798, -25.44774858730800560 ) ) ;
#5602 = DIRECTION ( 'NONE',  ( -0.5000000000000054401, 0.8660254037844354880, -0.000000000000000000 ) ) ;
#5603 = CARTESIAN_POINT ( 'NONE',  ( 229.6060668553226947, 37.02602910422319837, -15.48400627342739888 ) ) ;
#5604 = VECTOR ( 'NONE', #7997, 1000.000000000000000 ) ;
#5605 = ADVANCED_FACE ( 'NONE', ( #6526 ), #14838, .F. ) ;
#5606 = CARTESIAN_POINT ( 'NONE',  ( -28.12331899344885500, 75.90505089108978609, 3.056606027158062400 ) ) ;
#5607 = DIRECTION ( 'NONE',  ( -0.8660254037844354880, -0.5000000000000055511, 0.000000000000000000 ) ) ;
#5608 = CARTESIAN_POINT ( 'NONE',  ( 229.3261223513948721, 36.53144131726288890, -12.46964089162990064 ) ) ;
#5609 = CIRCLE ( 'NONE', #16129, 7.960520131757807150 ) ;
#5610 = ORIENTED_EDGE ( 'NONE', *, *, #7821, .F. ) ;
#5611 = VECTOR ( 'NONE', #11972, 1000.000000000000114 ) ;
#5612 = CARTESIAN_POINT ( 'NONE',  ( 78.05328906524978549, 56.09831538232894843, -3.025823995327163729 ) ) ;
#5613 = EDGE_CURVE ( 'NONE', #10227, #20099, #17306, .T. ) ;
#5614 = ORIENTED_EDGE ( 'NONE', *, *, #2694, .F. ) ;
#5615 = LINE ( 'NONE', #12210, #7450 ) ;
#5616 = DIRECTION ( 'NONE',  ( -0.000000000000000000, 4.625929269271485914E-16, -1.000000000000000000 ) ) ;
#5617 = EDGE_CURVE ( 'NONE', #13972, #2239, #4743, .T. ) ;
#5618 = AXIS2_PLACEMENT_3D ( 'NONE', #10529, #17115, #17014 ) ;
#5619 = CARTESIAN_POINT ( 'NONE',  ( 219.5629955745448285, 35.93464521499033282, -17.48830818005195908 ) ) ;
#5620 = EDGE_CURVE ( 'NONE', #18365, #3298, #9611, .T. ) ;
#5621 = VERTEX_POINT ( 'NONE', #14527 ) ;
#5622 = AXIS2_PLACEMENT_3D ( 'NONE', #6116, #20541, #13998 ) ;
#5623 = CARTESIAN_POINT ( 'NONE',  ( 76.76433846554481022, 54.31953569828399964, -19.93927737394622213 ) ) ;
#5624 = CARTESIAN_POINT ( 'NONE',  ( 226.3952283206526772, 41.60789869010848463, -10.82724490084729929 ) ) ;
#5625 = DIRECTION ( 'NONE',  ( 0.8660254037844370423, 0.5000000000000026645, -0.000000000000000000 ) ) ;
#5626 = CARTESIAN_POINT ( 'NONE',  ( -11.09026189855725164, 15.09941697557061957, 0.9457651797582804498 ) ) ;
#5627 = ORIENTED_EDGE ( 'NONE', *, *, #14702, .T. ) ;
#5628 = FACE_BOUND ( 'NONE', #16060, .T. ) ;
#5629 = EDGE_CURVE ( 'NONE', #13470, #18707, #11888, .T. ) ;
#5630 = FACE_OUTER_BOUND ( 'NONE', #17961, .T. ) ;
#5631 = DIRECTION ( 'NONE',  ( -0.8660254037844357100, -0.5000000000000051070, 0.000000000000000000 ) ) ;
#5632 = EDGE_LOOP ( 'NONE', ( #1624, #11668, #192, #1021, #8427, #13723 ) ) ;
#5633 = PRESENTATION_STYLE_ASSIGNMENT (( #13618 ) ) ;
#5634 = DIRECTION ( 'NONE',  ( -1.632680918566406547E-16, 1.632680918566406547E-16, -1.000000000000000000 ) ) ;
#5635 = CIRCLE ( 'NONE', #9021, 3.902363844300875240 ) ;
#5636 = DIRECTION ( 'NONE',  ( -1.000000000000000000, 0.000000000000000000, 0.000000000000000000 ) ) ;
#5637 = EDGE_CURVE ( 'NONE', #1337, #8365, #7087, .T. ) ;
#5638 = FACE_OUTER_BOUND ( 'NONE', #20459, .T. ) ;
#5639 = EDGE_CURVE ( 'NONE', #17136, #3819, #6442, .T. ) ;
#5641 = ORIENTED_EDGE ( 'NONE', *, *, #15032, .T. ) ;
#5640 = EDGE_LOOP ( 'NONE', ( #10838, #7014, #11294 ) ) ;
#5642 = VERTEX_POINT ( 'NONE', #13231 ) ;
#5643 = CARTESIAN_POINT ( 'NONE',  ( 209.3577037357181894, 3.480325248439696040, -14.00000000000005507 ) ) ;
#5644 = CARTESIAN_POINT ( 'NONE',  ( 226.5850146482969762, 42.25864501911018323, -16.29291827778581236 ) ) ;
#5645 = EDGE_CURVE ( 'NONE', #10243, #14630, #1072, .T. ) ;
#5646 = CARTESIAN_POINT ( 'NONE',  ( 208.8577037357181894, 4.346350652224124644, -14.00000000000005507 ) ) ;
#5647 = CARTESIAN_POINT ( 'NONE',  ( -29.99999999999999645, 5.000000000000000888, 3.748555621732009069 ) ) ;
#5648 =( NAMED_UNIT ( * ) PLANE_ANGLE_UNIT ( ) SI_UNIT ( $, .RADIAN. ) );
#5649 = CARTESIAN_POINT ( 'NONE',  ( 219.5332756341046547, 10.61828660343948272, -18.44761907388206623 ) ) ;
#5650 = ORIENTED_EDGE ( 'NONE', *, *, #9084, .F. ) ;
#5651 = AXIS2_PLACEMENT_3D ( 'NONE', #7372, #925, #6958 ) ;
#5652 = CARTESIAN_POINT ( 'NONE',  ( 82.93675860350933249, 62.01530615766962029, -25.34918193670429076 ) ) ;
#5653 = DIRECTION ( 'NONE',  ( 0.8660254037844360431, 0.5000000000000045519, 4.336808689942049784E-16 ) ) ;
#5654 = EDGE_CURVE ( 'NONE', #18696, #20283, #11220, .T. ) ;
#5655 = AXIS2_PLACEMENT_3D ( 'NONE', #5553, #12043, #3980 ) ;
#5656 = VERTEX_POINT ( 'NONE', #9915 ) ;
#5657 = DIRECTION ( 'NONE',  ( -0.4979466032338565329, 0.8624688162573705963, 0.09053574604251182767 ) ) ;
#5658 = LINE ( 'NONE', #13739, #18544 ) ;
#5659 = DIRECTION ( 'NONE',  ( 1.000000000000000000, 0.000000000000000000, -1.224646799147353207E-16 ) ) ;
#5660 = DIRECTION ( 'NONE',  ( -0.8660254037844370423, -0.5000000000000027756, -0.000000000000000000 ) ) ;
#5661 = CARTESIAN_POINT ( 'NONE',  ( 226.5660535422584019, 42.29148661813671595, -16.31968669809488759 ) ) ;
#5663 = VERTEX_POINT ( 'NONE', #11323 ) ;
#5662 = ORIENTED_EDGE ( 'NONE', *, *, #18498, .T. ) ;
#5664 = VERTEX_POINT ( 'NONE', #188 ) ;
#5665 = CARTESIAN_POINT ( 'NONE',  ( 221.7337709185422625, 32.16992198990818963, -13.98365758669818248 ) ) ;
#5666 = EDGE_CURVE ( 'NONE', #1146, #14093, #12904, .T. ) ;
#5667 = CARTESIAN_POINT ( 'NONE',  ( 57.15554463217811332, 244.9600622137188850, -13.99999999999998046 ) ) ;
#5668 = VERTEX_POINT ( 'NONE', #5153 ) ;
#5669 = AXIS2_PLACEMENT_3D ( 'NONE', #16802, #686, #15848 ) ;
#5670 = DIRECTION ( 'NONE',  ( 0.000000000000000000, -0.5000000000000008882, -0.8660254037844380415 ) ) ;
#5671 = CIRCLE ( 'NONE', #15200, 6.099999999999999645 ) ;
#5672 = PRODUCT ( 'Base Lock Knob', 'Base Lock Knob', '', ( #2781 ) ) ;
#5673 = DIRECTION ( 'NONE',  ( -0.000000000000000000, 4.625929269271485914E-16, -1.000000000000000000 ) ) ;
#5674 = DIRECTION ( 'NONE',  ( 0.7739085681710340392, 0.4468163201617105229, -0.4487991802004632214 ) ) ;
#5675 = CARTESIAN_POINT ( 'NONE',  ( 67.36131599811847082, 209.2831476774790360, 11.00000000000001066 ) ) ;
#5676 = CARTESIAN_POINT ( 'NONE',  ( -16.18016922445852046, 71.61437827766147279, -4.999999999999992895 ) ) ;
#5677 = ORIENTED_EDGE ( 'NONE', *, *, #19471, .T. ) ;
#5678 = CARTESIAN_POINT ( 'NONE',  ( 82.49529059433407951, 181.0703347563770365, 6.000000000000009770 ) ) ;
#5679 = EDGE_CURVE ( 'NONE', #19959, #20444, #19276, .T. ) ;
#5680 = CARTESIAN_POINT ( 'NONE',  ( 227.9553588074475954, 39.88513931160571957, -14.00000000000005507 ) ) ;
#5681 = CARTESIAN_POINT ( 'NONE',  ( -27.50943688352612782, 50.00306753912056479, -13.03837235451981336 ) ) ;
#5682 = PLANE ( 'NONE',  #2487 ) ;
#5683 = CARTESIAN_POINT ( 'NONE',  ( 61.99529059433388767, 216.5773763115390693, 1.000000000000017097 ) ) ;
#5684 = CARTESIAN_POINT ( 'NONE',  ( 199.2655634166889911, -1.083282501143478793, -21.18305361806749332 ) ) ;
#5686 = ORIENTED_EDGE ( 'NONE', *, *, #478, .T. ) ;
#5685 = EDGE_LOOP ( 'NONE', ( #18408, #2649, #17236 ) ) ;
#5687 = DIRECTION ( 'NONE',  ( -0.5000000000000049960, 0.8660254037844357100, -0.000000000000000000 ) ) ;
#5688 = CARTESIAN_POINT ( 'NONE',  ( 61.57468973143931379, 74.87077495648827608, -20.95977551465545119 ) ) ;
#5689 = EDGE_LOOP ( 'NONE', ( #5558, #10487 ) ) ;
#5690 = VERTEX_POINT ( 'NONE', #15968 ) ;
#5691 = ORIENTED_EDGE ( 'NONE', *, *, #2704, .T. ) ;
#5692 = CYLINDRICAL_SURFACE ( 'NONE', #10502, 4.999999999999973355 ) ;
#5693 = DIRECTION ( 'NONE',  ( -0.5000000000000047740, 0.8660254037844358210, 0.000000000000000000 ) ) ;
#5694 = AXIS2_PLACEMENT_3D ( 'NONE', #17303, #2887, #5938 ) ;
#5695 = EDGE_LOOP ( 'NONE', ( #11684, #20029, #18149, #17226 ) ) ;
#5696 = VERTEX_POINT ( 'NONE', #10857 ) ;
#5697 = EDGE_CURVE ( 'NONE', #15357, #2200, #16289, .T. ) ;
#5698 = LINE ( 'NONE', #15289, #3618 ) ;
#5699 = EDGE_LOOP ( 'NONE', ( #12754, #13679, #12738, #7060, #2298 ) ) ;
#5700 = LINE ( 'NONE', #20448, #3648 ) ;
#5701 = DIRECTION ( 'NONE',  ( -0.8660254037844360431, -0.5000000000000044409, 5.976026924694052093E-17 ) ) ;
#5702 = CARTESIAN_POINT ( 'NONE',  ( -11.66788315198026638, 17.61676080837512970, 11.72685522487003951 ) ) ;
#5703 = ADVANCED_FACE ( 'NONE', ( #1436 ), #19036, .F. ) ;
#5704 = CARTESIAN_POINT ( 'NONE',  ( 69.50490953756755630, 173.5703347563769796, 6.000000000000010658 ) ) ;
#5705 = DIRECTION ( 'NONE',  ( 0.8944271909999147452, 0.000000000000000000, -0.4472135954999602592 ) ) ;
#5706 = CARTESIAN_POINT ( 'NONE',  ( 199.1738290307970374, -1.136245373532171588, -9.972943347741736630 ) ) ;
#5707 = ORIENTED_EDGE ( 'NONE', *, *, #7586, .F. ) ;
#5708 = CARTESIAN_POINT ( 'NONE',  ( 177.1791022559528983, 56.75747545832872731, -29.00000000000007105 ) ) ;
#5709 = DIRECTION ( 'NONE',  ( -1.000000000000000000, 0.000000000000000000, 0.000000000000000000 ) ) ;
#5710 = CARTESIAN_POINT ( 'NONE',  ( 208.0983737146324870, 5.661548828456886895, -14.00000000000005507 ) ) ;
#5711 = AXIS2_PLACEMENT_3D ( 'NONE', #11649, #6640, #14949 ) ;
#5712 = ORIENTED_EDGE ( 'NONE', *, *, #576, .T. ) ;
#5713 = CARTESIAN_POINT ( 'NONE',  ( -0.1767699604045824824, 65.74999999999997158, 2.481238266578629226 ) ) ;
#5714 = ORIENTED_EDGE ( 'NONE', *, *, #12001, .F. ) ;
#5715 = DIRECTION ( 'NONE',  ( -0.5000000000000025535, 0.8660254037844372643, 0.000000000000000000 ) ) ;
#5716 = LINE ( 'NONE', #8703, #864 ) ;
#5717 = EDGE_CURVE ( 'NONE', #6944, #997, #11177, .T. ) ;
#5718 = APPLICATION_PROTOCOL_DEFINITION ( 'draft international standard', 'automotive_design', 1998, #2287 ) ;
#5719 = DIRECTION ( 'NONE',  ( -0.1503837331804321054, -0.08682408883346430517, 0.9848077530122086864 ) ) ;
#5720 = AXIS2_PLACEMENT_3D ( 'NONE', #1658, #9695, #17360 ) ;
#5721 = ORIENTED_EDGE ( 'NONE', *, *, #19864, .T. ) ;
#5722 = CARTESIAN_POINT ( 'NONE',  ( 202.6226596002730389, 0.8549378841442712984, -23.57241037536569195 ) ) ;
#5723 = VECTOR ( 'NONE', #7987, 1000.000000000000000 ) ;
#5724 = CARTESIAN_POINT ( 'NONE',  ( 205.5965122587965084, 9.994899983462953941, -14.00000000000005507 ) ) ;
#5725 = CARTESIAN_POINT ( 'NONE',  ( 220.7478146111253920, 34.29434874923224896, -17.58494696003844027 ) ) ;
#5726 = DIRECTION ( 'NONE',  ( -0.8296432542242783148, -0.4789947561577510560, -0.2868032327110804358 ) ) ;
#5727 = EDGE_CURVE ( 'NONE', #11917, #10920, #6327, .T. ) ;
#5728 = AXIS2_PLACEMENT_3D ( 'NONE', #9077, #18947, #10886 ) ;
#5729 = ADVANCED_FACE ( 'NONE', ( #3125 ), #14284, .T. ) ;
#5730 = CARTESIAN_POINT ( 'NONE',  ( 44.00000000000000000, 0.000000000000000000, -15.00000000000000355 ) ) ;
#5731 = AXIS2_PLACEMENT_3D ( 'NONE', #6170, #4593, #12551 ) ;
#5732 = CARTESIAN_POINT ( 'NONE',  ( 227.6776097244820392, 39.38674894399466808, -10.10863206319042362 ) ) ;
#5733 = DIRECTION ( 'NONE',  ( -0.8645602258681710506, -0.4991540791356393614, 0.05814482891047953461 ) ) ;
#5734 = ORIENTED_EDGE ( 'NONE', *, *, #218, .F. ) ;
#5735 = DIRECTION ( 'NONE',  ( 0.6123724356957914727, 0.3535533905932749521, -0.7071067811865495711 ) ) ;
#5736 = EDGE_CURVE ( 'NONE', #13841, #3757, #16072, .T. ) ;
#5737 = FACE_OUTER_BOUND ( 'NONE', #4469, .T. ) ;
#5738 = DIRECTION ( 'NONE',  ( 0.000000000000000000, -0.6846849967427295347, -0.7288391147814505810 ) ) ;
#5740 = EDGE_LOOP ( 'NONE', ( #5175, #18566, #14082, #13221, #3538, #20278 ) ) ;
#5739 = ORIENTED_EDGE ( 'NONE', *, *, #20218, .T. ) ;
#5741 = ORIENTED_EDGE ( 'NONE', *, *, #10661, .T. ) ;
#5742 = VECTOR ( 'NONE', #5978, 1000.000000000000114 ) ;
#5743 = PLANE ( 'NONE',  #7162 ) ;
#5744 = DIRECTION ( 'NONE',  ( -0.2300325188655851505, 0.3984280100682299208, 0.8878852184023702243 ) ) ;
#5745 = ORIENTED_EDGE ( 'NONE', *, *, #18305, .F. ) ;
#5746 = CARTESIAN_POINT ( 'NONE',  ( -16.93678575793154550, 80.00001702024998451, -12.48679740715397379 ) ) ;
#5747 = UNCERTAINTY_MEASURE_WITH_UNIT (LENGTH_MEASURE( 1.000000000000000082E-05 ), #17535, 'distance_accuracy_value', 'NONE');
#5748 = EDGE_CURVE ( 'NONE', #7006, #10440, #11546, .T. ) ;
#5749 = CARTESIAN_POINT ( 'NONE',  ( 227.5312376355471145, 39.64027283883993391, -14.00000000000005507 ) ) ;
#5750 = LINE ( 'NONE', #15550, #16856 ) ;
#5751 = DIRECTION ( 'NONE',  ( -0.8660254037844355990, -0.5000000000000054401, 4.435979565408006148E-14 ) ) ;
#5752 = AXIS2_PLACEMENT_3D ( 'NONE', #3707, #8160, #10161 ) ;
#5753 = ORIENTED_EDGE ( 'NONE', *, *, #3804, .T. ) ;
#5754 = EDGE_CURVE ( 'NONE', #20505, #8555, #2413, .T. ) ;
#5755 = CARTESIAN_POINT ( 'NONE',  ( 198.3351478706185276, -1.493051479916005730, -13.98983052576385866 ) ) ;
#5756 = AXIS2_PLACEMENT_3D ( 'NONE', #12400, #9083, #940 ) ;
#5757 = DIRECTION ( 'NONE',  ( -0.5000000000000054401, 0.8660254037844354880, -0.000000000000000000 ) ) ;
#5758 = VECTOR ( 'NONE', #14729, 1000.000000000000227 ) ;
#5759 = EDGE_LOOP ( 'NONE', ( #13009, #18702, #13212, #8419 ) ) ;
#5760 = LINE ( 'NONE', #6459, #10507 ) ;
#5761 = CARTESIAN_POINT ( 'NONE',  ( 190.7433706042750146, 35.72129598111152404, -19.00000000000003908 ) ) ;
#5762 = ADVANCED_FACE ( 'NONE', ( #4607 ), #17440, .F. ) ;
#5763 = AXIS2_PLACEMENT_3D ( 'NONE', #6220, #18960, #20440 ) ;
#5764 = EDGE_CURVE ( 'NONE', #2325, #15204, #1124, .T. ) ;
#5765 = CARTESIAN_POINT ( 'NONE',  ( 61.99529059433388767, 216.5773763115390693, -28.99999999999998934 ) ) ;
#5766 = PLANE ( 'NONE',  #3060 ) ;
#5767 = CARTESIAN_POINT ( 'NONE',  ( 228.0528179502890964, 39.71633512454245363, -17.56803216753791475 ) ) ;
#5768 = EDGE_CURVE ( 'NONE', #20411, #8176, #43, .T. ) ;
#5769 = ORIENTED_EDGE ( 'NONE', *, *, #10182, .T. ) ;
#5770 = ORIENTED_EDGE ( 'NONE', *, *, #2675, .F. ) ;
#5771 = CARTESIAN_POINT ( 'NONE',  ( 227.9553588074475954, 39.88513931160571957, -14.00000000000005507 ) ) ;
#5772 = CARTESIAN_POINT ( 'NONE',  ( 226.6211368133091923, 39.11482588413117867, -14.00000000000005507 ) ) ;
#5773 = AXIS2_PLACEMENT_3D ( 'NONE', #16712, #17603, #2190 ) ;
#5774 = VECTOR ( 'NONE', #12852, 1000.000000000000114 ) ;
#5775 = ORIENTED_EDGE ( 'NONE', *, *, #4376, .F. ) ;
#5776 = EDGE_LOOP ( 'NONE', ( #7416, #1022, #12887, #14631 ) ) ;
#5777 = DIRECTION ( 'NONE',  ( 0.8660254037844355990, 0.5000000000000054401, 1.074925455818303755E-13 ) ) ;
#5778 = CARTESIAN_POINT ( 'NONE',  ( 45.89721438298043665, 238.4600622137188282, -13.99999999999998046 ) ) ;
#5779 = AXIS2_PLACEMENT_3D ( 'NONE', #12653, #7960, #20377 ) ;
#5780 = VECTOR ( 'NONE', #14933, 1000.000000000000114 ) ;
#5781 = DIRECTION ( 'NONE',  ( -0.8660254037844361541, -0.5000000000000044409, 0.000000000000000000 ) ) ;
#5782 = ADVANCED_FACE ( 'NONE', ( #19338 ), #17546, .T. ) ;
#5783 = AXIS2_PLACEMENT_3D ( 'NONE', #574, #20173, #5636 ) ;
#5784 = CARTESIAN_POINT ( 'NONE',  ( 210.1178786253386193, 12.07426281049857408, -2.551678190571530891 ) ) ;
#5785 = LINE ( 'NONE', #12279, #12104 ) ;
#5786 = ORIENTED_EDGE ( 'NONE', *, *, #13010, .F. ) ;
#5787 = CARTESIAN_POINT ( 'NONE',  ( 229.5566283700793520, 36.45869994001149905, -14.55116774096007859 ) ) ;
#5788 = EDGE_CURVE ( 'NONE', #1032, #20933, #4122, .T. ) ;
#5789 = AXIS2_PLACEMENT_3D ( 'NONE', #483, #2176, #6922 ) ;
#5790 = PRESENTATION_STYLE_ASSIGNMENT (( #17363 ) ) ;
#5791 = CARTESIAN_POINT ( 'NONE',  ( -24.31754996354614207, 49.87382451390904237, -9.352669984570907147 ) ) ;
#5792 = CARTESIAN_POINT ( 'NONE',  ( 201.1037701599415755, 22.13968577106347269, -1.717498466822861225 ) ) ;
#5793 = VECTOR ( 'NONE', #15795, 1000.000000000000114 ) ;
#5794 = DIRECTION ( 'NONE',  ( -0.5000000000000041078, 0.8660254037844363761, 0.000000000000000000 ) ) ;
#5795 = CIRCLE ( 'NONE', #12254, 4.999999999999995559 ) ;
#5796 = DIRECTION ( 'NONE',  ( 1.000000000000000000, 0.000000000000000000, 0.000000000000000000 ) ) ;
#5798 = ORIENTED_EDGE ( 'NONE', *, *, #6374, .F. ) ;
#5797 = ORIENTED_EDGE ( 'NONE', *, *, #11749, .F. ) ;
#5799 = CARTESIAN_POINT ( 'NONE',  ( 203.0531299009467148, 24.20278031722661183, -13.00893198973463960 ) ) ;
#5800 =( REPRESENTATION_RELATIONSHIP ('NONE','NONE', #4634, #9759 ) REPRESENTATION_RELATIONSHIP_WITH_TRANSFORMATION ( #433 )SHAPE_REPRESENTATION_RELATIONSHIP( ) );
#5801 = FACE_BOUND ( 'NONE', #8961, .T. ) ;
#5802 = CARTESIAN_POINT ( 'NONE',  ( 228.1971211027353377, 38.48692884174984385, -10.33191597617941504 ) ) ;
#5803 = VERTEX_POINT ( 'NONE', #6187 ) ;
#5804 = ORIENTED_EDGE ( 'NONE', *, *, #195, .F. ) ;
#5805 = PLANE ( 'NONE',  #1036 ) ;
#5806 = CARTESIAN_POINT ( 'NONE',  ( 1.425125561529466012, 54.47798152960064755, -1.780651232228821046 ) ) ;
#5807 = CARTESIAN_POINT ( 'NONE',  ( 159.9952905943348469, 46.83639716978957068, 0.9999999999999386047 ) ) ;
#5808 = VERTEX_POINT ( 'NONE', #18923 ) ;
#5809 = VERTEX_POINT ( 'NONE', #12573 ) ;
#5810 = DIRECTION ( 'NONE',  ( -0.000000000000000000, 1.000000000000000000, -0.000000000000000000 ) ) ;
#5811 = EDGE_LOOP ( 'NONE', ( #20591, #9670, #12240, #1868 ) ) ;
#5812 = B_SPLINE_CURVE_WITH_KNOTS ( 'NONE', 3,
 ( #3003, #16243, #1417, #4990, #11155, #15944, #13071, #4897, #9445, #17631, #7867, #19513, #19617, #3404, #14367, #11468, #17944, #5093, #14680, #9758, #11368, #9857, #16354, #20795, #33, #6264, #6573, #12756, #16055, #1824, #134, #7966, #8270, #17842, #3309, #3110, #12971, #19218, #11271, #17740, #14781, #235, #9558, #4689, #6675, #1719, #1518, #14468, #20891, #13172, #17526, #6366, #12862, #19316 ),
 .UNSPECIFIED., .F., .F.,
 ( 4, 2, 2, 2, 2, 2, 2, 2, 2, 2, 2, 2, 2, 2, 2, 2, 2, 2, 2, 2, 2, 2, 2, 2, 2, 2, 4 ),
 ( 0.03645627031100262538, 0.03721136074309028957, 0.03796645117517795376, 0.03872154160726561795, 0.03947663203935328213, 0.04098681290352861051, 0.04174190333561626082, 0.04249699376770391113, 0.04551735549605451236, 0.04853771722440511360, 0.05155807895275570096, 0.05457844068110630220, 0.06061916413780750468, 0.06363952586615809204, 0.06665988759450866552, 0.06968024932285923900, 0.07119043018703451187, 0.07270061105120978473, 0.07345570148329741422, 0.07421079191538507147, 0.07496588234747270096, 0.07572097277956035821, 0.07723115364373561720, 0.07874133450791087618, 0.08176169623626142191, 0.08327187710043668090, 0.08478205796461193988 ),
 .UNSPECIFIED. ) ;
#5813 = AXIS2_PLACEMENT_3D ( 'NONE', #18777, #4250, #18983 ) ;
#5814 = VECTOR ( 'NONE', #7564, 1000.000000000000227 ) ;
#5815 = CARTESIAN_POINT ( 'NONE',  ( 220.2180084519553134, 35.41797800104779270, -14.00000000000005507 ) ) ;
#5816 = CARTESIAN_POINT ( 'NONE',  ( 218.7131701895986851, 37.40658595927892094, -16.57782486433068669 ) ) ;
#5817 = DIRECTION ( 'NONE',  ( 0.000000000000000000, -0.000000000000000000, 1.000000000000000000 ) ) ;
#5818 = AXIS2_PLACEMENT_3D ( 'NONE', #15325, #13818, #20068 ) ;
#5819 = CARTESIAN_POINT ( 'NONE',  ( 62.00490953756744972, 186.5607158131434744, 26.00000000000001776 ) ) ;
#5820 = LINE ( 'NONE', #2662, #12052 ) ;
#5821 = CARTESIAN_POINT ( 'NONE',  ( 127.2868417743716094, 73.48909236273162549, -18.99999999999997513 ) ) ;
#5822 = LINE ( 'NONE', #10598, #19548 ) ;
#5823 = CARTESIAN_POINT ( 'NONE',  ( 219.2413117866406083, 36.90368818298597375, -17.35168776101943777 ) ) ;
#5824 = DIRECTION ( 'NONE',  ( -0.8660254037844362651, -0.5000000000000042188, 6.872020471724002955E-17 ) ) ;
#5825 = ORIENTED_EDGE ( 'NONE', *, *, #3981, .T. ) ;
#5826 = VECTOR ( 'NONE', #12443, 1000.000000000000114 ) ;
#5827 = CARTESIAN_POINT ( 'NONE',  ( 82.07917159011968522, 61.14026859234759570, -0.08095729490022955666 ) ) ;
#5828 = B_SPLINE_CURVE_WITH_KNOTS ( 'NONE', 3,
 ( #4241, #5496, #10689, #11987 ),
 .UNSPECIFIED., .F., .F.,
 ( 4, 4 ),
 ( 7.412987158543330987E-07, 0.0005862296544554727396 ),
 .UNSPECIFIED. ) ;
#5829 = VECTOR ( 'NONE', #19756, 1000.000000000000000 ) ;
#5830 = VERTEX_POINT ( 'NONE', #4398 ) ;
#5831 = ORIENTED_EDGE ( 'NONE', *, *, #20924, .F. ) ;
#5832 = CARTESIAN_POINT ( 'NONE',  ( 5.000000000000000000, 4.685197434473812983, -6.938893903907228378E-15 ) ) ;
#5833 = CARTESIAN_POINT ( 'NONE',  ( 5.000000000000000000, 2.342598717236900718, -4.057500000000001883 ) ) ;
#5834 = EDGE_CURVE ( 'NONE', #6959, #13646, #10877, .T. ) ;
#5835 = CARTESIAN_POINT ( 'NONE',  ( 0.000000000000000000, 0.000000000000000000, 0.000000000000000000 ) ) ;
#5836 = DIRECTION ( 'NONE',  ( -0.2483788854152946257, -0.1434016163555414947, 0.9579895123154918979 ) ) ;
#5837 = ORIENTED_EDGE ( 'NONE', *, *, #16586, .T. ) ;
#5838 = CARTESIAN_POINT ( 'NONE',  ( 45.00000000000000000, -10.00000000000000000, -15.00000000000000000 ) ) ;
#5839 = CARTESIAN_POINT ( 'NONE',  ( 226.2189894626636431, 42.89261923747692862, -12.97935860811656816 ) ) ;
#5840 = FACE_BOUND ( 'NONE', #15435, .T. ) ;
#5841 = CARTESIAN_POINT ( 'NONE',  ( 208.0983737146324870, 5.661548828456886895, -14.00000000000005507 ) ) ;
#5842 = LINE ( 'NONE', #19006, #4500 ) ;
#5843 = EDGE_CURVE ( 'NONE', #2929, #13343, #6814, .T. ) ;
#5844 = DIRECTION ( 'NONE',  ( -0.5000000000000055511, 0.8660254037844354880, 0.000000000000000000 ) ) ;
#5845 = CARTESIAN_POINT ( 'NONE',  ( 205.5965122587965084, 9.994899983462952164, -14.00000000000005507 ) ) ;
#5846 = CARTESIAN_POINT ( 'NONE',  ( 205.3906008270068071, 3.225829587143459243, -2.044871543906942701 ) ) ;
#5847 = PRODUCT_DEFINITION_SHAPE ( 'NONE', 'NONE',  #20955 ) ;
#5848 = ORIENTED_EDGE ( 'NONE', *, *, #7327, .F. ) ;
#5849 = CARTESIAN_POINT ( 'NONE',  ( -3.649238679178553380, 77.92717739396518084, 2.017250382391169605 ) ) ;
#5850 = CARTESIAN_POINT ( 'NONE',  ( 220.1860095456201236, 35.06147156406766641, -10.32863559915725915 ) ) ;
#5851 = CARTESIAN_POINT ( 'NONE',  ( 5.000000000000004441, 3.513898075855358183, 2.028750000000009379 ) ) ;
#5852 = VECTOR ( 'NONE', #6163, 1000.000000000000114 ) ;
#5853 = EDGE_CURVE ( 'NONE', #3287, #4912, #407, .T. ) ;
#5855 = ORIENTED_EDGE ( 'NONE', *, *, #17705, .T. ) ;
#5854 = EDGE_LOOP ( 'NONE', ( #11800, #2721, #15594, #20249, #2415 ) ) ;
#5856 = ADVANCED_FACE ( 'NONE', ( #6811 ), #6473, .T. ) ;
#5857 = CARTESIAN_POINT ( 'NONE',  ( 221.7368532287422909, 32.37533151030277168, -12.57085682670548721 ) ) ;
#5858 =( NAMED_UNIT ( * ) SI_UNIT ( $, .STERADIAN. ) SOLID_ANGLE_UNIT ( ) );
#5859 = VERTEX_POINT ( 'NONE', #5010 ) ;
#5860 = CARTESIAN_POINT ( 'NONE',  ( -35.00000000000000000, 64.25000000000000000, -1.525597966176003961 ) ) ;
#5861 = CARTESIAN_POINT ( 'NONE',  ( 0.3999999999999975797, 0.000000000000000000, 0.000000000000000000 ) ) ;
#5862 = CARTESIAN_POINT ( 'NONE',  ( 220.3053218761288861, 33.13539195642835011, -16.94731950718130875 ) ) ;
#5863 = B_SPLINE_CURVE_WITH_KNOTS ( 'NONE', 3,
 ( #4473, #16877, #1297, #16038 ),
 .UNSPECIFIED., .F., .F.,
 ( 4, 4 ),
 ( 4.612368003688608817E-05, 0.0006120499023169649958 ),
 .UNSPECIFIED. ) ;
#5864 = ADVANCED_FACE ( 'NONE', ( #3221 ), #4138, .T. ) ;
#5865 = CARTESIAN_POINT ( 'NONE',  ( 227.8354303126693594, 40.09286155783686212, -17.89498551959672312 ) ) ;
#5866 = CIRCLE ( 'NONE', #14025, 4.999999999999976907 ) ;
#5867 = AXIS2_PLACEMENT_3D ( 'NONE', #3509, #6777, #5290 ) ;
#5868 = SHAPE_REPRESENTATION_RELATIONSHIP ( 'NONE' , 'NONE' ,  #10571, #12383 ) ;
#5869 = EDGE_LOOP ( 'NONE', ( #10504, #2513, #11648, #5955 ) ) ;
#5870 = DIRECTION ( 'NONE',  ( 0.000000000000000000, -1.000000000000000000, 0.000000000000000000 ) ) ;
#5871 = CARTESIAN_POINT ( 'NONE',  ( -4.705817999896520831, 64.80165467510407495, 5.356440324370162820 ) ) ;
#5872 = EDGE_CURVE ( 'NONE', #17011, #2714, #6067, .T. ) ;
#5873 = DIRECTION ( 'NONE',  ( 0.8660254037844417052, -0.4999999999999947820, 1.060575238724906422E-16 ) ) ;
#5874 = FACE_OUTER_BOUND ( 'NONE', #9901, .T. ) ;
#5875 = FACE_OUTER_BOUND ( 'NONE', #711, .T. ) ;
#5876 = ORIENTED_EDGE ( 'NONE', *, *, #15032, .F. ) ;
#5877 = ORIENTED_EDGE ( 'NONE', *, *, #18975, .T. ) ;
#5878 = CARTESIAN_POINT ( 'NONE',  ( 220.8087949685757394, 32.26335098006651947, -12.10162843130820676 ) ) ;
#5879 = EDGE_CURVE ( 'NONE', #2754, #16112, #19846, .T. ) ;
#5880 = VERTEX_POINT ( 'NONE', #5732 ) ;
#5881 = DIRECTION ( 'NONE',  ( -0.1017280065263192340, 0.1761980758562746441, -0.9790840876823234673 ) ) ;
#5882 = CARTESIAN_POINT ( 'NONE',  ( 79.36047190431955300, 49.50000000000057554, -12.02697745110878280 ) ) ;
#5883 = CARTESIAN_POINT ( 'NONE',  ( 32.39721438298033007, 261.8427481158985302, -22.00000000000000355 ) ) ;
#5884 = CIRCLE ( 'NONE', #17754, 11.98469917212512215 ) ;
#5885 = CARTESIAN_POINT ( 'NONE',  ( 5.000000000000000000, 5.258101095580057891E-15, 4.057499999999999218 ) ) ;
#5886 = EDGE_CURVE ( 'NONE', #14632, #18333, #14649, .T. ) ;
#5887 = ORIENTED_EDGE ( 'NONE', *, *, #16146, .F. ) ;
#5888 = EDGE_CURVE ( 'NONE', #16315, #7807, #8824, .T. ) ;
#5889 = FACE_OUTER_BOUND ( 'NONE', #1534, .T. ) ;
#5890 = PLANE ( 'NONE',  #16334 ) ;
#5891 = CARTESIAN_POINT ( 'NONE',  ( -22.79285140204124716, 49.64535697708226536, -10.50220247801678752 ) ) ;
#5892 = CYLINDRICAL_SURFACE ( 'NONE', #2822, 3.902363844300889451 ) ;
#5893 = VECTOR ( 'NONE', #5208, 1000.000000000000000 ) ;
#5894 = ADVANCED_FACE ( 'NONE', ( #5630 ), #13614, .T. ) ;
#5895 = CARTESIAN_POINT ( 'NONE',  ( 196.8823445864675534, 4.963772932080226852, -7.502777792348571673 ) ) ;
#5896 = CARTESIAN_POINT ( 'NONE',  ( 229.6822319185971253, 36.89410734487046284, -14.91677899116121431 ) ) ;
#5898 = EDGE_LOOP ( 'NONE', ( #19191, #19908, #12731, #8617 ) ) ;
#5897 = VERTEX_POINT ( 'NONE', #4052 ) ;
#5899 = CARTESIAN_POINT ( 'NONE',  ( 218.9852377222535154, 11.07469685814948157, -16.89203719259520753 ) ) ;
#5900 = CARTESIAN_POINT ( 'NONE',  ( 44.99529059433372424, 246.0222400402097946, -8.999999999999973355 ) ) ;
#5901 = ORIENTED_EDGE ( 'NONE', *, *, #11594, .F. ) ;
#5902 = EDGE_LOOP ( 'NONE', ( #18095, #16975, #745, #16401 ) ) ;
#5903 = CARTESIAN_POINT ( 'NONE',  ( 205.0662616026534693, 10.91332106064940888, -14.00000000000005507 ) ) ;
#5904 = CARTESIAN_POINT ( 'NONE',  ( 200.8894739819445192, 11.40128808463920329, -25.34310559273323804 ) ) ;
#5905 = CARTESIAN_POINT ( 'NONE',  ( -32.78929790297351587, 51.06562928705771753, -6.895168070231495250 ) ) ;
#5906 = CARTESIAN_POINT ( 'NONE',  ( 62.36389338619030553, 105.9389375482328006, -29.00000000000000000 ) ) ;
#5907 = ADVANCED_FACE ( 'NONE', ( #11803 ), #881, .T. ) ;
#5908 = ORIENTED_EDGE ( 'NONE', *, *, #1252, .F. ) ;
#5909 = ORIENTED_EDGE ( 'NONE', *, *, #6121, .T. ) ;
#5910 = CARTESIAN_POINT ( 'NONE',  ( 219.3753053876406511, 36.25973415479045059, -17.38313153181858084 ) ) ;
#5911 = ORIENTED_EDGE ( 'NONE', *, *, #10029, .F. ) ;
#5912 = EDGE_CURVE ( 'NONE', #11034, #11090, #669, .T. ) ;
#5913 = CARTESIAN_POINT ( 'NONE',  ( 221.1877743307729531, 33.12044585814464881, -16.57782486433075775 ) ) ;
#5914 = SPHERICAL_SURFACE ( 'NONE', #2181, 12.00000000000002665 ) ;
#5915 = AXIS2_PLACEMENT_3D ( 'NONE', #392, #14826, #16297 ) ;
#5916 = CARTESIAN_POINT ( 'NONE',  ( -11.16353062760892634, 16.40948116617020958, 11.52664465621722734 ) ) ;
#5917 = ADVANCED_FACE ( 'NONE', ( #12227 ), #18708, .T. ) ;
#5918 = CARTESIAN_POINT ( 'NONE',  ( 5.000000000000004441, 2.342598717236856309, 4.057500000000020535 ) ) ;
#5919 = DIRECTION ( 'NONE',  ( 0.5000000000000049960, -0.8660254037844358210, 0.000000000000000000 ) ) ;
#5920 = CARTESIAN_POINT ( 'NONE',  ( 191.5478494775925640, 36.18576207517880050, -14.00000000000006395 ) ) ;
#5921 = APPLICATION_CONTEXT ( 'automotive_design' ) ;
#5922 = VERTEX_POINT ( 'NONE', #18266 ) ;
#5923 = DIRECTION ( 'NONE',  ( 0.000000000000000000, -1.000000000000000000, 0.000000000000000000 ) ) ;
#5924 = DIRECTION ( 'NONE',  ( -0.5000000000000045519, 0.8660254037844360431, 4.006172263299081054E-16 ) ) ;
#5925 = CARTESIAN_POINT ( 'NONE',  ( -11.59722103597593801, 11.66854079980773129, 3.430876175762954006 ) ) ;
#5926 = ORIENTED_EDGE ( 'NONE', *, *, #14356, .T. ) ;
#5927 = CLOSED_SHELL ( 'NONE', ( #12509, #8115, #8098, #1896, #8560, #6051, #11221, #4731, #14582, #16267, #7579, #4198, #13178, #13707, #13696, #17936, #19015, #13259, #19429, #12566, #1749, #6884, #18238, #719 ) ) ;
#5928 = CARTESIAN_POINT ( 'NONE',  ( 81.62617710402389548, 62.35908199265414709, 0.2316258051034030541 ) ) ;
#5929 = ORIENTED_EDGE ( 'NONE', *, *, #11454, .F. ) ;
#5930 = AXIS2_PLACEMENT_3D ( 'NONE', #17098, #16989, #4478 ) ;
#5931 = ORIENTED_EDGE ( 'NONE', *, *, #3923, .T. ) ;
#5932 = CARTESIAN_POINT ( 'NONE',  ( -0.1767699604045824824, 64.25000000000000000, 2.481238266578627449 ) ) ;
#5933 = AXIS2_PLACEMENT_3D ( 'NONE', #11262, #3196, #6253 ) ;
#5934 = DIRECTION ( 'NONE',  ( -1.000000000000000000, 0.000000000000000000, 0.000000000000000000 ) ) ;
#5935 = PRODUCT_CONTEXT ( 'NONE', #15314, 'mechanical' ) ;
#5936 = LINE ( 'NONE', #12436, #11988 ) ;
#5937 = FACE_OUTER_BOUND ( 'NONE', #12258, .T. ) ;
#5938 = DIRECTION ( 'NONE',  ( 0.5000000000000041078, -0.8660254037844363761, 0.000000000000000000 ) ) ;
#5939 = DIRECTION ( 'NONE',  ( 0.5000000000000046629, -0.8660254037844360431, 0.000000000000000000 ) ) ;
#5940 = CARTESIAN_POINT ( 'NONE',  ( 205.0662616026534693, 10.91332106064940888, -14.00000000000005507 ) ) ;
#5941 = AXIS2_PLACEMENT_3D ( 'NONE', #10361, #18335, #5693 ) ;
#5942 = ORIENTED_EDGE ( 'NONE', *, *, #19125, .F. ) ;
#5943 = LINE ( 'NONE', #15529, #5826 ) ;
#5944 = VECTOR ( 'NONE', #3045, 1000.000000000000000 ) ;
#5945 = DIRECTION ( 'NONE',  ( 0.5000000000000051070, -0.8660254037844359321, 0.000000000000000000 ) ) ;
#5946 = PLANE ( 'NONE',  #19654 ) ;
#5947 = EDGE_CURVE ( 'NONE', #19425, #3223, #20268, .T. ) ;
#5948 = DIRECTION ( 'NONE',  ( 0.2961981327260175823, 0.1710100716628329964, -0.9396926207859105373 ) ) ;
#5949 = ORIENTED_EDGE ( 'NONE', *, *, #2123, .T. ) ;
#5950 = DIRECTION ( 'NONE',  ( -0.7951984747223580507, -0.4591080534401394408, 0.3960797660391671138 ) ) ;
#5951 = DIRECTION ( 'NONE',  ( -0.8660254037844355990, -0.5000000000000054401, 0.000000000000000000 ) ) ;
#5952 = AXIS2_PLACEMENT_3D ( 'NONE', #18367, #244, #6685 ) ;
#5953 = CYLINDRICAL_SURFACE ( 'NONE', #3443, 9.999999999999994671 ) ;
#5954 = CARTESIAN_POINT ( 'NONE',  ( 227.8089867185128412, 40.13866320645101382, -9.756613004592562532 ) ) ;
#5956 = VERTEX_POINT ( 'NONE', #10399 ) ;
#5955 = ORIENTED_EDGE ( 'NONE', *, *, #2618, .T. ) ;
#5957 = VECTOR ( 'NONE', #17242, 1000.000000000000114 ) ;
#5958 = DIRECTION ( 'NONE',  ( 0.5000000000000054401, -0.8660254037844354880, 0.000000000000000000 ) ) ;
#5959 = CARTESIAN_POINT ( 'NONE',  ( 23.43933576707516053, 253.3582490066810919, 32.55737704917950737 ) ) ;
#5960 = AXIS2_PLACEMENT_3D ( 'NONE', #14793, #11908, #13186 ) ;
#5961 = ORIENTED_EDGE ( 'NONE', *, *, #5316, .F. ) ;
#5962 = UNCERTAINTY_MEASURE_WITH_UNIT (LENGTH_MEASURE( 1.000000000000000082E-05 ), #19886, 'distance_accuracy_value', 'NONE');
#5963 = ADVANCED_FACE ( 'NONE', ( #568 ), #18694, .F. ) ;
#5964 = B_SPLINE_CURVE_WITH_KNOTS ( 'NONE', 3,
 ( #4271, #20690, #12652, #15141 ),
 .UNSPECIFIED., .F., .F.,
 ( 4, 4 ),
 ( 1.346642366733436829E-06, 0.0004533998841465750724 ),
 .UNSPECIFIED. ) ;
#5965 = CARTESIAN_POINT ( 'NONE',  ( 221.4641624591582172, 32.64172757717244622, -12.10162843130820853 ) ) ;
#5966 = CARTESIAN_POINT ( 'NONE',  ( 5.000000000000000000, -2.342598717236899386, 4.057500000000001883 ) ) ;
#5967 = CARTESIAN_POINT ( 'NONE',  ( 201.4752803508637271, 7.615505632025055149, -24.99940654434229970 ) ) ;
#5968 = ORIENTED_EDGE ( 'NONE', *, *, #9109, .F. ) ;
#5969 = DIRECTION ( 'NONE',  ( -0.7951984747223626027, -0.4591080534401424385, -0.3960797660391544017 ) ) ;
#5970 = EDGE_CURVE ( 'NONE', #4222, #11795, #3131, .T. ) ;
#5971 = VERTEX_POINT ( 'NONE', #17101 ) ;
#5972 = DIRECTION ( 'NONE',  ( 0.000000000000000000, 0.8108848540793840431, -0.5852057359806516201 ) ) ;
#5973 = CIRCLE ( 'NONE', #15486, 5.000000000000008882 ) ;
#5974 = EDGE_CURVE ( 'NONE', #9470, #5187, #4837, .T. ) ;
#5975 = DIRECTION ( 'NONE',  ( 0.5943026915289566503, 0.3431208189343674109, -0.7273736415730548410 ) ) ;
#5976 = FACE_OUTER_BOUND ( 'NONE', #14051, .T. ) ;
#5977 = CYLINDRICAL_SURFACE ( 'NONE', #1693, 5.999999999999998224 ) ;
#5978 = DIRECTION ( 'NONE',  ( 0.5566703992264184775, 0.3213938048432737893, 0.7660444431189769032 ) ) ;
#5979 = ORIENTED_EDGE ( 'NONE', *, *, #2807, .F. ) ;
#5980 = VERTEX_POINT ( 'NONE', #11915 ) ;
#5981 = FACE_BOUND ( 'NONE', #4282, .T. ) ;
#5982 = ORIENTED_EDGE ( 'NONE', *, *, #977, .T. ) ;
#5983 = LINE ( 'NONE', #18732, #6498 ) ;
#5984 = CARTESIAN_POINT ( 'NONE',  ( 227.0194864344331904, 40.85315867856421335, -10.42293161028223025 ) ) ;
#5985 = DIRECTION ( 'NONE',  ( -0.7739085681710340392, -0.4468163201617105229, 0.4487991802004632214 ) ) ;
#5986 = DIRECTION ( 'NONE',  ( 0.8660254037844355990, 0.5000000000000054401, 9.734124438199387596E-15 ) ) ;
#5987 = AXIS2_PLACEMENT_3D ( 'NONE', #8021, #16316, #13031 ) ;
#5988 = LINE ( 'NONE', #4722, #18556 ) ;
#5989 = ORIENTED_EDGE ( 'NONE', *, *, #1391, .T. ) ;
#5990 = AXIS2_PLACEMENT_3D ( 'NONE', #18663, #7728, #18875 ) ;
#5991 = CARTESIAN_POINT ( 'NONE',  ( 57.20986367771982373, 224.8659788670219655, 44.53282986889902162 ) ) ;
#5992 = EDGE_CURVE ( 'NONE', #9600, #15844, #15003, .T. ) ;
#5993 = EDGE_CURVE ( 'NONE', #15249, #13448, #9029, .T. ) ;
#5994 = CARTESIAN_POINT ( 'NONE',  ( 219.0819991370609330, 37.38560385231634342, -10.82724490084729929 ) ) ;
#5995 = CARTESIAN_POINT ( 'NONE',  ( -22.24814625259552869, 45.17694441447353881, -10.83184487622254899 ) ) ;
#5996 = CARTESIAN_POINT ( 'NONE',  ( 198.6508758837858579, -1.438172513732599578, -19.95367855226118436 ) ) ;
#5997 = CARTESIAN_POINT ( 'NONE',  ( 219.2049426021622764, 11.20154352970703471, -12.53629070788368338 ) ) ;
#5998 = CARTESIAN_POINT ( 'NONE',  ( -27.50045467171848301, 45.80088190002059889, -4.911061130343635561 ) ) ;
#5999 = VECTOR ( 'NONE', #3342, 1000.000000000000000 ) ;
#6000 = B_SPLINE_CURVE_WITH_KNOTS ( 'NONE', 3,
 ( #2160, #10397, #11802, #3628 ),
 .UNSPECIFIED., .F., .F.,
 ( 4, 4 ),
 ( 1.854400302564232594E-06, 0.0008558401382852200449 ),
 .UNSPECIFIED. ) ;
#6002 = ORIENTED_EDGE ( 'NONE', *, *, #5727, .T. ) ;
#6001 = VERTEX_POINT ( 'NONE', #10293 ) ;
#6003 = CARTESIAN_POINT ( 'NONE',  ( 85.37797649651368204, 230.0773763115391262, -28.99999999999998934 ) ) ;
#6004 = CARTESIAN_POINT ( 'NONE',  ( 5.000000000000000000, -2.342598717236899386, 4.057500000000001883 ) ) ;
#6005 = VECTOR ( 'NONE', #19010, 1000.000000000000000 ) ;
#6006 = CARTESIAN_POINT ( 'NONE',  ( 1.204513484672493639, 77.44204738084411588, -4.113378397035853062 ) ) ;
#6007 = VERTEX_POINT ( 'NONE', #15530 ) ;
#6008 = EDGE_CURVE ( 'NONE', #14393, #17982, #7231, .T. ) ;
#6009 = DIRECTION ( 'NONE',  ( 0.000000000000000000, 0.000000000000000000, -1.000000000000000000 ) ) ;
#6010 = LINE ( 'NONE', #1366, #2065 ) ;
#6011 = CARTESIAN_POINT ( 'NONE',  ( -33.40960586970430768, 54.51484073799145591, -1.766275756695815380 ) ) ;
#6012 = CARTESIAN_POINT ( 'NONE',  ( -27.39744768730504987, 9.624020198635008683, 5.177064134126243111 ) ) ;
#6013 = B_SPLINE_CURVE_WITH_KNOTS ( 'NONE', 3,
 ( #5261, #13239, #1998, #19686 ),
 .UNSPECIFIED., .F., .F.,
 ( 4, 4 ),
 ( 0.0001336956365395343524, 0.0008063464285820690254 ),
 .UNSPECIFIED. ) ;
#6014 = ORIENTED_EDGE ( 'NONE', *, *, #12550, .F. ) ;
#6015 = ORIENTED_EDGE ( 'NONE', *, *, #5768, .F. ) ;
#6016 = CARTESIAN_POINT ( 'NONE',  ( 4.000000000000000000, -3.518949890710766581, 4.553649124439118623E-15 ) ) ;
#6017 = ORIENTED_EDGE ( 'NONE', *, *, #17179, .T. ) ;
#6018 = ADVANCED_FACE ( 'NONE', ( #3733 ), #11557, .T. ) ;
#6019 = DIRECTION ( 'NONE',  ( 0.5000000000000045519, -0.8660254037844360431, -0.000000000000000000 ) ) ;
#6020 = AXIS2_PLACEMENT_3D ( 'NONE', #3095, #15929, #6248 ) ;
#6021 = VECTOR ( 'NONE', #7627, 999.9999999999998863 ) ;
#6022 = CARTESIAN_POINT ( 'NONE',  ( 229.4896559907413689, 37.22765863623112637, -12.08027307405518869 ) ) ;
#6023 = CARTESIAN_POINT ( 'NONE',  ( 69.76445162107610543, 76.82718752816320773, -23.28021896557464387 ) ) ;
#6024 = EDGE_CURVE ( 'NONE', #14936, #16542, #17733, .T. ) ;
#6025 =( GEOMETRIC_REPRESENTATION_CONTEXT ( 3 ) GLOBAL_UNCERTAINTY_ASSIGNED_CONTEXT ( ( #8277 ) ) GLOBAL_UNIT_ASSIGNED_CONTEXT ( ( #15806, #4550, #11229 ) ) REPRESENTATION_CONTEXT ( 'NONE', 'WORKASPACE' ) );
#6026 = DIRECTION ( 'NONE',  ( -1.000000000000000000, -0.000000000000000000, -0.000000000000000000 ) ) ;
#6027 = DIRECTION ( 'NONE',  ( -0.5943026915289653100, -0.3431208189343725179, -0.7273736415730454041 ) ) ;
#6028 = CARTESIAN_POINT ( 'NONE',  ( 225.5801007209566365, 43.01974110743358182, -13.97349461567471707 ) ) ;
#6029 = ORIENTED_EDGE ( 'NONE', *, *, #14641, .F. ) ;
#6030 = CARTESIAN_POINT ( 'NONE',  ( 208.4761278624580711, 5.007259451653140125, -14.00000000000005507 ) ) ;
#6031 = DIRECTION ( 'NONE',  ( 0.8660254037844355990, 0.5000000000000054401, -2.642119490368404866E-15 ) ) ;
#6032 = CYLINDRICAL_SURFACE ( 'NONE', #1394, 8.000000000000058620 ) ;
#6033 = VERTEX_POINT ( 'NONE', #7433 ) ;
#6034 = CARTESIAN_POINT ( 'NONE',  ( 79.10508859364674095, 67.76772306032525250, 0.2307413371220972953 ) ) ;
#6035 = EDGE_CURVE ( 'NONE', #12385, #9708, #4147, .T. ) ;
#6036 = ORIENTED_EDGE ( 'NONE', *, *, #20170, .F. ) ;
#6037 = ADVANCED_FACE ( 'NONE', ( #15634 ), #12340, .F. ) ;
#6038 = CIRCLE ( 'NONE', #13851, 11.98469917212512215 ) ;
#6039 = ORIENTED_EDGE ( 'NONE', *, *, #7836, .T. ) ;
#6040 = CARTESIAN_POINT ( 'NONE',  ( -3.541693527980152023, 79.08610913872911397, 1.260722419662599236 ) ) ;
#6041 = LINE ( 'NONE', #1082, #13743 ) ;
#6042 = SHAPE_DEFINITION_REPRESENTATION ( #9067, #3951 ) ;
#6043 = EDGE_CURVE ( 'NONE', #4595, #3334, #6164, .T. ) ;
#6044 = LINE ( 'NONE', #20258, #10261 ) ;
#6045 = ORIENTED_EDGE ( 'NONE', *, *, #18884, .F. ) ;
#6046 = DIRECTION ( 'NONE',  ( -0.8660254037844360431, -0.5000000000000045519, -4.336808689942049784E-16 ) ) ;
#6047 = CARTESIAN_POINT ( 'NONE',  ( 196.1289531908403490, 19.26747385478372721, -2.044871543906938705 ) ) ;
#6048 = CARTESIAN_POINT ( 'NONE',  ( 229.7218892158732615, 36.82541889109744204, -14.53509620734055829 ) ) ;
#6049 = VECTOR ( 'NONE', #14453, 1000.000000000000114 ) ;
#6050 = CARTESIAN_POINT ( 'NONE',  ( 228.5632073782796851, 38.17935557111412237, -17.36588157897878304 ) ) ;
#6051 = ADVANCED_FACE ( 'NONE', ( #4486 ), #19009, .T. ) ;
#6052 = B_SPLINE_CURVE_WITH_KNOTS ( 'NONE', 3,
 ( #18369, #4042, #20060, #20156, #8710, #18259, #13497, #3725, #3943, #5522, #8816, #11691, #15317, #10075, #2359, #2047, #13706, #773, #13287, #7224, #15002, #13606, #5623, #15209, #3835, #8391, #5204, #10181, #5305, #16879, #660, #8500, #16987, #10498, #10286, #12110, #16673, #11796, #18576, #12010, #19943, #5411, #14893, #8605, #354, #460, #6801, #18157, #2155, #15102 ),
 .UNSPECIFIED., .F., .F.,
 ( 4, 2, 2, 2, 2, 2, 2, 2, 2, 2, 2, 2, 2, 2, 2, 2, 2, 2, 2, 2, 2, 2, 2, 2, 4 ),
 ( 0.1153743516471457259, 0.1159013919239667845, 0.1164284322007878569, 0.1169554724776089155, 0.1174825127544299741, 0.1185365933080721051, 0.1195906738617142223, 0.1216988349689984705, 0.1238069960762827049, 0.1259151571835669670, 0.1280233182908512013, 0.1301314793981354634, 0.1322396405054196977, 0.1332937210590618149, 0.1343478016127039598, 0.1364559627199881942, 0.1375100432736303391, 0.1385641238272724562, 0.1406722849345567183, 0.1417263654881988355, 0.1427804460418409527, 0.1448886071491252148, 0.1459426877027673319, 0.1469967682564094491, 0.1491049293636936834 ),
 .UNSPECIFIED. ) ;
#6053 = CARTESIAN_POINT ( 'NONE',  ( 82.49529059433407951, 181.0703347563770365, 16.00000000000001066 ) ) ;
#6054 = CARTESIAN_POINT ( 'NONE',  ( 191.5936596622672141, 35.49346171468950928, -9.029101044830413869 ) ) ;
#6055 = CARTESIAN_POINT ( 'NONE',  ( 210.6527207509366519, 17.03810123488167605, -3.480441514389755575 ) ) ;
#6056 = ORIENTED_EDGE ( 'NONE', *, *, #10790, .F. ) ;
#6057 = CARTESIAN_POINT ( 'NONE',  ( 195.4946457851292507, 4.162584655573419390, -16.75125533358848884 ) ) ;
#6058 = DIRECTION ( 'NONE',  ( -0.4999999999999995004, 0.8660254037844390407, 0.000000000000000000 ) ) ;
#6059 = FACE_OUTER_BOUND ( 'NONE', #8108, .T. ) ;
#6060 = DIRECTION ( 'NONE',  ( -1.218100516808353647E-16, 9.146065988991504310E-17, -1.000000000000000000 ) ) ;
#6062 = ORIENTED_EDGE ( 'NONE', *, *, #8091, .T. ) ;
#6061 = ORIENTED_EDGE ( 'NONE', *, *, #561, .F. ) ;
#6063 = ORIENTED_EDGE ( 'NONE', *, *, #8198, .F. ) ;
#6064 = AXIS2_PLACEMENT_3D ( 'NONE', #2080, #14820, #6508 ) ;
#6065 = CARTESIAN_POINT ( 'NONE',  ( 5.000000000000000000, -4.685197434473809430, 6.071532165918824830E-15 ) ) ;
#6066 = SURFACE_STYLE_USAGE ( .BOTH. , #13726 ) ;
#6067 = B_SPLINE_CURVE_WITH_KNOTS ( 'NONE', 3,
 ( #19531, #17959, #11385, #16466, #14798, #1638, #9973, #19431, #17862, #13297, #16169, #2055, #3530, #8078, #1950, #250, #8399, #14900, #19743, #9776, #3329, #6489, #8512, #16261, #1742, #5212, #15011, #149, #3428, #8189, #14695, #13090, #6695, #11701, #50, #364, #6590, #10083, #5114, #11485, #9877, #6912, #16370, #14587, #18165, #12986, #1847, #16573, #468, #13193, #13397, #11598 ),
 .UNSPECIFIED., .F., .F.,
 ( 4, 2, 2, 2, 2, 2, 2, 2, 2, 2, 2, 2, 2, 2, 2, 2, 2, 2, 2, 2, 2, 2, 2, 2, 2, 4 ),
 ( 0.04446192691180363837, 0.04521014590794605881, 0.04595836490408848618, 0.04745480289637336868, 0.04895124088865825118, 0.05044767888094312674, 0.05344055486551287093, 0.05643343085008261512, 0.06241918281922204104, 0.06541205880379177828, 0.06840493478836148777, 0.07139781077293121114, 0.07439068675750092063, 0.07588712474978578926, 0.07738356274207063012, 0.07813178173821305750, 0.07888000073435547099, 0.08037643872664032574, 0.08112465772278276699, 0.08187287671892518048, 0.08262109571506760786, 0.08336931471121003523, 0.08486575270349486222, 0.08636219069577970309, 0.08935506668034937094, 0.09234794266491903880 ),
 .UNSPECIFIED. ) ;
#6068 = CARTESIAN_POINT ( 'NONE',  ( 208.8107687779841228, 4.427644383670616079, -14.00000000000005507 ) ) ;
#6069 = CARTESIAN_POINT ( 'NONE',  ( 196.7914626300884322, 9.035300127502988943, -22.62267072728657169 ) ) ;
#6070 = CARTESIAN_POINT ( 'NONE',  ( 178.2433706042749009, 57.37193107572242923, -14.00000000000002842 ) ) ;
#6071 = AXIS2_PLACEMENT_3D ( 'NONE', #4992, #1827, #3407 ) ;
#6072 = FACE_OUTER_BOUND ( 'NONE', #2848, .T. ) ;
#6073 = VECTOR ( 'NONE', #3626, 1000.000000000000000 ) ;
#6074 = ORIENTED_EDGE ( 'NONE', *, *, #4294, .T. ) ;
#6075 = CARTESIAN_POINT ( 'NONE',  ( -15.99999999999999289, 0.000000000000000000, 0.000000000000000000 ) ) ;
#6076 = LINE ( 'NONE', #14283, #4981 ) ;
#6077 = AXIS2_PLACEMENT_3D ( 'NONE', #7257, #5659, #18611 ) ;
#6078 = CYLINDRICAL_SURFACE ( 'NONE', #329, 13.99999999999999822 ) ;
#6079 = FACE_OUTER_BOUND ( 'NONE', #4416, .T. ) ;
#6080 = VECTOR ( 'NONE', #2636, 1000.000000000000227 ) ;
#6081 = ORIENTED_EDGE ( 'NONE', *, *, #1227, .T. ) ;
#6082 = ORIENTED_EDGE ( 'NONE', *, *, #17593, .T. ) ;
#6083 = PLANE ( 'NONE',  #382 ) ;
#6084 = B_SPLINE_CURVE_WITH_KNOTS ( 'NONE', 3,
 ( #19301, #19403, #11140, #19199 ),
 .UNSPECIFIED., .F., .F.,
 ( 4, 4 ),
 ( 2.916652380847781525E-07, 0.0006729424572906142791 ),
 .UNSPECIFIED. ) ;
#6085 = ORIENTED_EDGE ( 'NONE', *, *, #20526, .T. ) ;
#6086 = ORIENTED_EDGE ( 'NONE', *, *, #3467, .F. ) ;
#6087 = LINE ( 'NONE', #15464, #2474 ) ;
#6088 = DIRECTION ( 'NONE',  ( 1.000000000000000000, -0.000000000000000000, -0.000000000000000000 ) ) ;
#6089 = FACE_OUTER_BOUND ( 'NONE', #2679, .T. ) ;
#6090 = VECTOR ( 'NONE', #18060, 1000.000000000000227 ) ;
#6091 = LINE ( 'NONE', #9375, #17125 ) ;
#6092 = EDGE_CURVE ( 'NONE', #18827, #13693, #15964, .T. ) ;
#6093 = CIRCLE ( 'NONE', #349, 12.00000000000002487 ) ;
#6094 = ORIENTED_EDGE ( 'NONE', *, *, #6183, .T. ) ;
#6095 = AXIS2_PLACEMENT_3D ( 'NONE', #15016, #19850, #5216 ) ;
#6096 = FACE_OUTER_BOUND ( 'NONE', #5304, .T. ) ;
#6097 = AXIS2_PLACEMENT_3D ( 'NONE', #3691, #16221, #1697 ) ;
#6098 = CARTESIAN_POINT ( 'NONE',  ( 229.3155625773928250, 36.54973138235077812, -15.57898118447804769 ) ) ;
#6099 = CARTESIAN_POINT ( 'NONE',  ( -5.772503121411054039, 50.66968791804065830, -7.229964842171530570 ) ) ;
#6100 = DIRECTION ( 'NONE',  ( 0.8660254037844355990, 0.5000000000000054401, 0.000000000000000000 ) ) ;
#6101 = LINE ( 'NONE', #18848, #17608 ) ;
#6102 = AXIS2_PLACEMENT_3D ( 'NONE', #17621, #11145, #1405 ) ;
#6103 = CARTESIAN_POINT ( 'NONE',  ( -19.05307565254539526, 45.50731414553807497, -12.12761656432236279 ) ) ;
#6105 = ORIENTED_EDGE ( 'NONE', *, *, #6263, .T. ) ;
#6104 = VERTEX_POINT ( 'NONE', #10947 ) ;
#6106 = AXIS2_PLACEMENT_3D ( 'NONE', #17372, #2853, #9288 ) ;
#6107 = FACE_OUTER_BOUND ( 'NONE', #16086, .T. ) ;
#6108 = CARTESIAN_POINT ( 'NONE',  ( 198.1555906521723784, 9.822879808262255708, -2.579136038830115218 ) ) ;
#6109 = CARTESIAN_POINT ( 'NONE',  ( 0.8940010539731342298, 77.84073441274544791, -4.744404894158055441 ) ) ;
#6110 = CIRCLE ( 'NONE', #18645, 5.999999999999998224 ) ;
#6111 = ORIENTED_EDGE ( 'NONE', *, *, #7734, .F. ) ;
#6112 = EDGE_LOOP ( 'NONE', ( #3721, #554, #4698, #13492, #4436, #5481, #16637, #11954 ) ) ;
#6113 = DIRECTION ( 'NONE',  ( 0.5000000000000054401, -0.8660254037844354880, 0.000000000000000000 ) ) ;
#6114 = LINE ( 'NONE', #4231, #17642 ) ;
#6115 = CARTESIAN_POINT ( 'NONE',  ( -33.44495115927801976, 54.23679612179412146, -2.044894016340141896 ) ) ;
#6116 = CARTESIAN_POINT ( 'NONE',  ( 227.9553588074475670, 39.88513931160575510, -14.00000000000005507 ) ) ;
#6117 = ORIENTED_EDGE ( 'NONE', *, *, #16814, .T. ) ;
#6118 = EDGE_CURVE ( 'NONE', #6530, #3344, #17627, .T. ) ;
#6119 = AXIS2_PLACEMENT_3D ( 'NONE', #2425, #12290, #13767 ) ;
#6120 = EDGE_LOOP ( 'NONE', ( #15718, #18928, #1167, #18298 ) ) ;
#6121 = EDGE_CURVE ( 'NONE', #14524, #9834, #17416, .T. ) ;
#6122 = CARTESIAN_POINT ( 'NONE',  ( 227.9553588074475954, 39.88513931160571957, -14.00000000000005507 ) ) ;
#6123 = CARTESIAN_POINT ( 'NONE',  ( 194.9230649354363152, 18.57125394591359679, -2.551678190571418092 ) ) ;
#6124 = CIRCLE ( 'NONE', #8162, 5.999999999999998224 ) ;
#6125 = CARTESIAN_POINT ( 'NONE',  ( 209.9477407942357843, 12.50708294970442402, -13.58165309559974254 ) ) ;
#6126 = VECTOR ( 'NONE', #1412, 1000.000000000000000 ) ;
#6127 = CARTESIAN_POINT ( 'NONE',  ( 221.3116568450157899, 33.11179325011160302, -16.66317149659884223 ) ) ;
#6128 = CARTESIAN_POINT ( 'NONE',  ( 64.92628429094538944, 80.60227088397526529, -21.04771496906974804 ) ) ;
#6129 = AXIS2_PLACEMENT_3D ( 'NONE', #10628, #4388, #17323 ) ;
#6130 = AXIS2_PLACEMENT_3D ( 'NONE', #18486, #5320, #7131 ) ;
#6131 = EDGE_CURVE ( 'NONE', #3430, #2720, #15854, .T. ) ;
#6132 = CARTESIAN_POINT ( 'NONE',  ( 227.6511661303252367, 39.43255059260894768, -17.89498551959673023 ) ) ;
#6133 = FACE_OUTER_BOUND ( 'NONE', #4442, .T. ) ;
#6134 = CARTESIAN_POINT ( 'NONE',  ( -19.76533548850507316, 18.40525104484276397, 11.92183032960170586 ) ) ;
#6135 = CIRCLE ( 'NONE', #6119, 5.400000000000001243 ) ;
#6136 = CARTESIAN_POINT ( 'NONE',  ( -31.93815604754423632, 67.52062497874923963, 2.295552037966095416 ) ) ;
#6137 = CARTESIAN_POINT ( 'NONE',  ( 214.5332756341045979, 19.27854064128383982, -18.44761907388206978 ) ) ;
#6138 = DIRECTION ( 'NONE',  ( -0.8660254037844372643, -0.5000000000000027756, 0.000000000000000000 ) ) ;
#6139 = EDGE_LOOP ( 'NONE', ( #15801, #14073, #13329, #6945, #19869 ) ) ;
#6141 = EDGE_CURVE ( 'NONE', #18407, #19279, #20475, .T. ) ;
#6140 = CARTESIAN_POINT ( 'NONE',  ( 79.29870457202490286, 66.51502123048413750, 0.4125900521836811663 ) ) ;
#6142 = ORIENTED_EDGE ( 'NONE', *, *, #9754, .T. ) ;
#6143 = ORIENTED_EDGE ( 'NONE', *, *, #12360, .F. ) ;
#6144 = DIRECTION ( 'NONE',  ( 1.000000000000000000, 0.000000000000000000, 0.000000000000000000 ) ) ;
#6145 = CONICAL_SURFACE ( 'NONE', #3108, 10.85470691220533190, 0.8171114040043576665 ) ;
#6146 = ADVANCED_FACE ( 'NONE', ( #12545 ), #5946, .F. ) ;
#6147 = VECTOR ( 'NONE', #7204, 1000.000000000000227 ) ;
#6148 = DIRECTION ( 'NONE',  ( -0.1997192025788217806, -0.1153079353712217758, -0.9730448705798236952 ) ) ;
#6149 = ORIENTED_EDGE ( 'NONE', *, *, #868, .F. ) ;
#6150 = APPLICATION_PROTOCOL_DEFINITION ( 'draft international standard', 'automotive_design', 1998, #12849 ) ;
#6151 = VECTOR ( 'NONE', #3844, 1000.000000000000227 ) ;
#6152 = DIRECTION ( 'NONE',  ( -0.5000000000000045519, 0.8660254037844360431, 0.000000000000000000 ) ) ;
#6153 = ORIENTED_EDGE ( 'NONE', *, *, #9749, .F. ) ;
#6154 = CARTESIAN_POINT ( 'NONE',  ( 28.51452848080066005, 214.5677573683055357, -8.999999999999969802 ) ) ;
#6155 = CARTESIAN_POINT ( 'NONE',  ( 209.2927537897656407, 30.87096182040829007, -15.98783141827518328 ) ) ;
#6156 = CARTESIAN_POINT ( 'NONE',  ( 0.1080579935186935236, 61.16269310544473825, 2.006079461162327160 ) ) ;
#6157 = EDGE_CURVE ( 'NONE', #19244, #19592, #9554, .T. ) ;
#6158 = EDGE_CURVE ( 'NONE', #8779, #9213, #19214, .T. ) ;
#6159 = CARTESIAN_POINT ( 'NONE',  ( -15.99999999999999289, 15.09941697557068530, 0.9999999999999991118 ) ) ;
#6160 = DIRECTION ( 'NONE',  ( 0.5000000000000051070, -0.8660254037844355990, -4.163336342344335178E-17 ) ) ;
#6161 = VECTOR ( 'NONE', #1195, 1000.000000000000114 ) ;
#6162 = CIRCLE ( 'NONE', #7861, 3.047499999999999876 ) ;
#6163 = DIRECTION ( 'NONE',  ( -0.1005394128318083530, -0.05804645706261224447, 0.9932383577419438003 ) ) ;
#6164 = LINE ( 'NONE', #4272, #6126 ) ;
#6165 = DIRECTION ( 'NONE',  ( 0.5000000000000026645, -0.8660254037844369313, 0.000000000000000000 ) ) ;
#6166 = ORIENTED_EDGE ( 'NONE', *, *, #6799, .F. ) ;
#6168 = ADVANCED_FACE ( 'NONE', ( #15737 ), #2894, .F. ) ;
#6167 = CARTESIAN_POINT ( 'NONE',  ( 225.6560297040601313, 42.88822825093131286, -12.92165662794185366 ) ) ;
#6169 = DIRECTION ( 'NONE',  ( 0.1997192025788092906, 0.1153079353712144900, -0.9730448705798270259 ) ) ;
#6170 = CARTESIAN_POINT ( 'NONE',  ( 208.8107687779841228, 4.427644383670616079, -14.00000000000005507 ) ) ;
#6171 = DIRECTION ( 'NONE',  ( -0.5000000000000049960, 0.8660254037844358210, -0.000000000000000000 ) ) ;
#6172 = CARTESIAN_POINT ( 'NONE',  ( -33.50112344255473573, 76.50873768553087473, -2.871813542385711848 ) ) ;
#6174 = VERTEX_POINT ( 'NONE', #12445 ) ;
#6173 = VERTEX_POINT ( 'NONE', #9335 ) ;
#6175 =( NAMED_UNIT ( * ) PLANE_ANGLE_UNIT ( ) SI_UNIT ( $, .RADIAN. ) );
#6176 = PRODUCT_DEFINITION_CONTEXT ( 'detailed design', #6880, 'design' ) ;
#6177 = ADVANCED_FACE ( 'NONE', ( #18904 ), #10829, .F. ) ;
#6178 = AXIS2_PLACEMENT_3D ( 'NONE', #5083, #11567, #8904 ) ;
#6179 = COLOUR_RGB ( '',0.7921568627450980005, 0.8196078431372548767, 0.9333333333333333481 ) ;
#6180 = LINE ( 'NONE', #12768, #1920 ) ;
#6181 = CARTESIAN_POINT ( 'NONE',  ( 218.2235991490363745, 38.25454787544715174, -14.91677899116112016 ) ) ;
#6182 = CARTESIAN_POINT ( 'NONE',  ( 226.5028411374610755, 42.40097371491420830, -17.10689588174065534 ) ) ;
#6183 = EDGE_CURVE ( 'NONE', #2667, #1597, #2795, .T. ) ;
#6184 = ORIENTED_EDGE ( 'NONE', *, *, #1593, .F. ) ;
#6185 = DIRECTION ( 'NONE',  ( -0.8660254037844378194, -0.5000000000000013323, -0.000000000000000000 ) ) ;
#6186 = EDGE_LOOP ( 'NONE', ( #9589, #20225, #8142 ) ) ;
#6187 = CARTESIAN_POINT ( 'NONE',  ( 44.00000000000000000, 0.000000000000000000, -15.00000000000000355 ) ) ;
#6188 = DIRECTION ( 'NONE',  ( -0.8660254037844355990, -0.5000000000000054401, -9.734124438199387596E-15 ) ) ;
#6189 = AXIS2_PLACEMENT_3D ( 'NONE', #13765, #8877, #20427 ) ;
#6190 = PLANE ( 'NONE',  #19624 ) ;
#6191 = CARTESIAN_POINT ( 'NONE',  ( 0.000000000000000000, -4.685197434473809430, 6.071532165918824830E-15 ) ) ;
#6192 = VERTEX_POINT ( 'NONE', #17522 ) ;
#6193 = CARTESIAN_POINT ( 'NONE',  ( 227.6158839122614097, 40.47312707796264419, -10.49174204642374697 ) ) ;
#6194 = ORIENTED_EDGE ( 'NONE', *, *, #11094, .F. ) ;
#6195 = ORIENTED_EDGE ( 'NONE', *, *, #1267, .T. ) ;
#6196 = CARTESIAN_POINT ( 'NONE',  ( 1.500000000000001332, 0.000000000000000000, 6.500000000000000888 ) ) ;
#6197 = DIRECTION ( 'NONE',  ( 0.9367698044638387289, 0.000000000000000000, -0.3499461864984122483 ) ) ;
#6198 = CARTESIAN_POINT ( 'NONE',  ( 226.4416686084753110, 42.50692764314508310, -12.10162843130810373 ) ) ;
#6199 = CARTESIAN_POINT ( 'NONE',  ( 209.6971420603676677, 12.36239970324706050, -2.990331769139234375 ) ) ;
#6200 = CARTESIAN_POINT ( 'NONE',  ( 200.4259095341650152, 0.1018498810115307518, -6.098918798390397633 ) ) ;
#6201 = VECTOR ( 'NONE', #15823, 1000.000000000000227 ) ;
#6202 = CIRCLE ( 'NONE', #10597, 12.47473710546057823 ) ;
#6203 = ORIENTED_EDGE ( 'NONE', *, *, #6679, .F. ) ;
#6204 = LINE ( 'NONE', #14506, #2700 ) ;
#6205 = CYLINDRICAL_SURFACE ( 'NONE', #5472, 12.47473710546057646 ) ;
#6206 = CARTESIAN_POINT ( 'NONE',  ( -1.904422244483446214, 50.06947204901834425, -10.93639821325584016 ) ) ;
#6207 = DIRECTION ( 'NONE',  ( 0.8660254037844380415, 0.5000000000000008882, 0.000000000000000000 ) ) ;
#6208 = CARTESIAN_POINT ( 'NONE',  ( 207.4817114093494297, 25.82199186828477266, -22.03054070023868860 ) ) ;
#6209 = CARTESIAN_POINT ( 'NONE',  ( -23.85050882933249738, 45.02920876159776498, -9.734908535650388828 ) ) ;
#6210 = EDGE_CURVE ( 'NONE', #15437, #1522, #2999, .T. ) ;
#6211 = ORIENTED_EDGE ( 'NONE', *, *, #6646, .F. ) ;
#6212 = VECTOR ( 'NONE', #5701, 1000.000000000000227 ) ;
#6213 = DIRECTION ( 'NONE',  ( 1.000000000000000000, 0.000000000000000000, 0.000000000000000000 ) ) ;
#6214 = LINE ( 'NONE', #3048, #11195 ) ;
#6215 = CARTESIAN_POINT ( 'NONE',  ( 228.9802228740807948, 38.11002267734541959, -16.98332657222556108 ) ) ;
#6216 = ORIENTED_EDGE ( 'NONE', *, *, #5494, .F. ) ;
#6217 = VERTEX_POINT ( 'NONE', #19611 ) ;
#6218 = ORIENTED_EDGE ( 'NONE', *, *, #6755, .F. ) ;
#6219 = FACE_OUTER_BOUND ( 'NONE', #19922, .T. ) ;
#6220 = CARTESIAN_POINT ( 'NONE',  ( 8.399999999999998579, 0.000000000000000000, 0.000000000000000000 ) ) ;
#6221 = CARTESIAN_POINT ( 'NONE',  ( -9.814647292144057289, 50.28451303171664222, -15.41809052414373049 ) ) ;
#6222 = DIRECTION ( 'NONE',  ( -0.8660254037844363761, -0.5000000000000041078, -0.000000000000000000 ) ) ;
#6223 = ORIENTED_EDGE ( 'NONE', *, *, #12130, .T. ) ;
#6224 = ORIENTED_EDGE ( 'NONE', *, *, #19740, .T. ) ;
#6225 = DIRECTION ( 'NONE',  ( 0.000000000000000000, 0.4999999999999985012, -0.8660254037844394848 ) ) ;
#6227 = ADVANCED_FACE ( 'NONE', ( #20888 ), #19312, .F. ) ;
#6226 =( NAMED_UNIT ( * ) PLANE_ANGLE_UNIT ( ) SI_UNIT ( $, .RADIAN. ) );
#6228 = AXIS2_PLACEMENT_3D ( 'NONE', #4393, #7347, #15551 ) ;
#6229 = CARTESIAN_POINT ( 'NONE',  ( 227.2894753402594006, 41.03848330869583805, -10.33191597617938484 ) ) ;
#6230 = SHAPE_REPRESENTATION ( 'socket head cap screw_iso_ISO 4762 M8 x 35 - 35N', ( #18233 ), #2321 ) ;
#6231 = LINE ( 'NONE', #17596, #16646 ) ;
#6232 = CARTESIAN_POINT ( 'NONE',  ( 203.7027818574982518, 1.478546760110915903, -24.25943249057081630 ) ) ;
#6233 = FACE_OUTER_BOUND ( 'NONE', #2825, .T. ) ;
#6234 = ADVANCED_FACE ( 'NONE', ( #334 ), #3510, .T. ) ;
#6235 = CARTESIAN_POINT ( 'NONE',  ( 219.1503276808599594, 36.64940697350503029, -10.80501622924627902 ) ) ;
#6236 = DIRECTION ( 'NONE',  ( 0.000000000000000000, 0.000000000000000000, 1.000000000000000000 ) ) ;
#6237 = CARTESIAN_POINT ( 'NONE',  ( -15.99999999999999289, 10.09941697557069418, 4.999999999999989342 ) ) ;
#6238 = EDGE_CURVE ( 'NONE', #16821, #5249, #12859, .T. ) ;
#6239 = ORIENTED_EDGE ( 'NONE', *, *, #1932, .T. ) ;
#6240 = CARTESIAN_POINT ( 'NONE',  ( 80.96799772285972097, 65.13527580443323473, 0.5013398903319724598 ) ) ;
#6241 = EDGE_LOOP ( 'NONE', ( #12708, #871, #2692, #14320 ) ) ;
#6242 = ORIENTED_EDGE ( 'NONE', *, *, #3290, .F. ) ;
#6243 = CARTESIAN_POINT ( 'NONE',  ( -0.06184395245637178823, 67.52062497875388658, 2.295552037965487013 ) ) ;
#6244 = LINE ( 'NONE', #19298, #1894 ) ;
#6245 = APPLICATION_PROTOCOL_DEFINITION ( 'draft international standard', 'automotive_design', 1998, #14096 ) ;
#6246 = CARTESIAN_POINT ( 'NONE',  ( 198.5374064076044078, -1.503684146350823703, -15.40190399002796440 ) ) ;
#6247 = ORIENTED_EDGE ( 'NONE', *, *, #4998, .T. ) ;
#6248 = DIRECTION ( 'NONE',  ( 0.000000000000000000, 0.000000000000000000, 1.000000000000000000 ) ) ;
#6249 = DIRECTION ( 'NONE',  ( 0.4999999999999995004, -0.8660254037844390407, 0.000000000000000000 ) ) ;
#6250 = DIRECTION ( 'NONE',  ( -0.8660254037844357100, -0.5000000000000051070, 0.000000000000000000 ) ) ;
#6251 = CARTESIAN_POINT ( 'NONE',  ( 227.2443279398389109, 41.11668090005410647, -18.00871210835852665 ) ) ;
#6252 = ADVANCED_FACE ( 'NONE', ( #3200 ), #17653, .T. ) ;
#6253 = DIRECTION ( 'NONE',  ( 0.5000000000000029976, -0.8660254037844370423, 0.000000000000000000 ) ) ;
#6254 = DIRECTION ( 'NONE',  ( -0.4999999999999995004, 0.8660254037844390407, 0.000000000000000000 ) ) ;
#6255 = EDGE_CURVE ( 'NONE', #4315, #14773, #19719, .T. ) ;
#6256 = DIRECTION ( 'NONE',  ( 0.5000000000000054401, -0.8660254037844353769, 2.220446049250312588E-16 ) ) ;
#6257 = DIRECTION ( 'NONE',  ( -0.5000000000000053291, 0.8660254037844354880, 0.000000000000000000 ) ) ;
#6258 = CIRCLE ( 'NONE', #18811, 12.50000000000000000 ) ;
#6259 = CARTESIAN_POINT ( 'NONE',  ( -11.10102051443364779, 16.09941697557071905, 0.9999999999999997780 ) ) ;
#6260 = EDGE_LOOP ( 'NONE', ( #17951, #10716, #7342, #11741 ) ) ;
#6261 = CIRCLE ( 'NONE', #7963, 12.47473710546057823 ) ;
#6262 = CARTESIAN_POINT ( 'NONE',  ( 220.7941474011230127, 33.80222769952564477, -17.14987233279968848 ) ) ;
#6263 = EDGE_CURVE ( 'NONE', #18877, #6425, #12168, .T. ) ;
#6264 = CARTESIAN_POINT ( 'NONE',  ( 74.48213423432167701, 73.05094370868849296, -0.3751272339344335349 ) ) ;
#6265 = CARTESIAN_POINT ( 'NONE',  ( 196.4296119619006618, 4.702387629415611947, -19.29168348739290195 ) ) ;
#6266 = DIRECTION ( 'NONE',  ( 0.000000000000000000, 0.000000000000000000, -1.000000000000000000 ) ) ;
#6267 = EDGE_CURVE ( 'NONE', #17471, #5980, #11463, .T. ) ;
#6268 = B_SPLINE_CURVE_WITH_KNOTS ( 'NONE', 3,
 ( #9509, #18004, #3472, #9916 ),
 .UNSPECIFIED., .F., .F.,
 ( 4, 4 ),
 ( 5.955297919795845203E-07, 0.0004526487715718483982 ),
 .UNSPECIFIED. ) ;
#6270 = EDGE_LOOP ( 'NONE', ( #8550, #16847, #4118, #350 ) ) ;
#6269 = VERTEX_POINT ( 'NONE', #13064 ) ;
#6271 = EDGE_CURVE ( 'NONE', #7814, #16010, #3843, .T. ) ;
#6272 = PLANE ( 'NONE',  #11247 ) ;
#6273 = CARTESIAN_POINT ( 'NONE',  ( 219.5629955745448285, 35.93464521499033282, -17.48830818005195908 ) ) ;
#6274 = EDGE_LOOP ( 'NONE', ( #6568, #19367, #8343, #6623, #16757, #13496 ) ) ;
#6275 = CIRCLE ( 'NONE', #18139, 3.619616396367202782 ) ;
#6276 = CARTESIAN_POINT ( 'NONE',  ( 228.1017308963825201, 39.63161541676043953, -10.10863206319042362 ) ) ;
#6277 = CONICAL_SURFACE ( 'NONE', #5594, 10.85470691220533190, 0.8171114040043576665 ) ;
#6278 = CARTESIAN_POINT ( 'NONE',  ( -27.95202372264500212, 79.14876326484322533, -7.307758369671589094 ) ) ;
#6279 = CARTESIAN_POINT ( 'NONE',  ( 195.3740178925880002, 3.738913527986503560, -11.16670872502617584 ) ) ;
#6280 = EDGE_CURVE ( 'NONE', #6599, #6373, #16238, .T. ) ;
#6281 = ORIENTED_EDGE ( 'NONE', *, *, #13154, .T. ) ;
#6282 = CARTESIAN_POINT ( 'NONE',  ( 208.0983737146324870, 5.661548828456886895, -14.00000000000005507 ) ) ;
#6283 = EDGE_CURVE ( 'NONE', #10758, #2805, #13930, .T. ) ;
#6284 = ORIENTED_EDGE ( 'NONE', *, *, #16667, .T. ) ;
#6285 = CARTESIAN_POINT ( 'NONE',  ( 199.6917776511935472, -0.3220013592427101723, -7.237580838289900953 ) ) ;
#6286 = DIRECTION ( 'NONE',  ( 0.5000000000000054401, -0.8660254037844354880, 0.000000000000000000 ) ) ;
#6287 = CIRCLE ( 'NONE', #20499, 5.000000000000000000 ) ;
#6288 = ADVANCED_FACE ( 'NONE', ( #19508 ), #3401, .F. ) ;
#6289 = CARTESIAN_POINT ( 'NONE',  ( 30.10683012259193703, 0.000000000000000000, 0.000000000000000000 ) ) ;
#6290 = DIRECTION ( 'NONE',  ( -0.4272097022732491700, 0.7399489098236288198, -0.5195839500354345608 ) ) ;
#6291 = VECTOR ( 'NONE', #6854, 1000.000000000000114 ) ;
#6292 = ORIENTED_EDGE ( 'NONE', *, *, #5639, .T. ) ;
#6293 = AXIS2_PLACEMENT_3D ( 'NONE', #6751, #2116, #421 ) ;
#6294 = DIRECTION ( 'NONE',  ( -0.8660254037844360431, -0.5000000000000044409, 0.000000000000000000 ) ) ;
#6295 = EDGE_CURVE ( 'NONE', #13147, #8980, #4860, .T. ) ;
#6296 = VERTEX_POINT ( 'NONE', #10061 ) ;
#6297 = CARTESIAN_POINT ( 'NONE',  ( 209.0110543411082062, 31.54257417018269649, -12.89263383701904608 ) ) ;
#6298 = CARTESIAN_POINT ( 'NONE',  ( 205.5965122587965084, 9.994899983462953941, -14.00000000000005507 ) ) ;
#6299 = CARTESIAN_POINT ( 'NONE',  ( 220.3379369467334925, 35.21025575481678516, -17.89498551959673023 ) ) ;
#6300 = ADVANCED_FACE ( 'NONE', ( #4893, #6567 ), #9853, .T. ) ;
#6301 = LINE ( 'NONE', #261, #6612 ) ;
#6302 = EDGE_CURVE ( 'NONE', #4567, #15885, #9658, .T. ) ;
#6303 = ORIENTED_EDGE ( 'NONE', *, *, #2153, .F. ) ;
#6304 = AXIS2_PLACEMENT_3D ( 'NONE', #12998, #12791, #4825 ) ;
#6305 = FACE_OUTER_BOUND ( 'NONE', #4952, .T. ) ;
#6306 = CARTESIAN_POINT ( 'NONE',  ( -5.637571478551725690, 50.76112637345350720, -7.048071971797520874 ) ) ;
#6307 = DIRECTION ( 'NONE',  ( 0.000000000000000000, 1.000000000000000000, -1.355657144061424088E-15 ) ) ;
#6308 = EDGE_CURVE ( 'NONE', #13300, #694, #17331, .T. ) ;
#6309 = B_SPLINE_CURVE_WITH_KNOTS ( 'NONE', 3,
 ( #12533, #14141, #2885, #5722 ),
 .UNSPECIFIED., .F., .F.,
 ( 4, 4 ),
 ( 3.854193985120393637E-07, 0.0008543711573788317915 ),
 .UNSPECIFIED. ) ;
#6310 = DIRECTION ( 'NONE',  ( -1.000000000000000000, 0.000000000000000000, 0.000000000000000000 ) ) ;
#6311 = CARTESIAN_POINT ( 'NONE',  ( 218.2478963529180191, 38.62433418721651179, -13.51727824498684072 ) ) ;
#6313 = ORIENTED_EDGE ( 'NONE', *, *, #14874, .F. ) ;
#6312 = ORIENTED_EDGE ( 'NONE', *, *, #15906, .T. ) ;
#6314 = VERTEX_POINT ( 'NONE', #4031 ) ;
#6315 = CARTESIAN_POINT ( 'NONE',  ( 4.000000000000000000, 0.000000000000000000, 0.000000000000000000 ) ) ;
#6316 = CARTESIAN_POINT ( 'NONE',  ( 227.9553588074475954, 39.88513931160571957, -14.00000000000005507 ) ) ;
#6317 = CARTESIAN_POINT ( 'NONE',  ( -12.43358389273065256, 79.99999999999585043, -11.99131545410286925 ) ) ;
#6318 = ORIENTED_EDGE ( 'NONE', *, *, #309, .T. ) ;
#6319 = AXIS2_PLACEMENT_3D ( 'NONE', #19282, #11228, #17697 ) ;
#6320 = DIRECTION ( 'NONE',  ( 0.5000000000000046629, -0.8660254037844359321, 0.000000000000000000 ) ) ;
#6321 = CARTESIAN_POINT ( 'NONE',  ( 195.2889461848653525, 4.043823935988862139, -15.40420431385919464 ) ) ;
#6322 = CARTESIAN_POINT ( 'NONE',  ( -32.43274721513416381, 59.32595788850117202, 1.390757872376907178 ) ) ;
#6323 = DIRECTION ( 'NONE',  ( -0.5000000000000008882, 0.8660254037844381525, 0.000000000000000000 ) ) ;
#6324 = ORIENTED_EDGE ( 'NONE', *, *, #11708, .F. ) ;
#6325 = ORIENTED_EDGE ( 'NONE', *, *, #3839, .F. ) ;
#6326 = CARTESIAN_POINT ( 'NONE',  ( -0.1286331481417117006, 66.76123571212174568, 2.404802591979303905 ) ) ;
#6327 = B_SPLINE_CURVE_WITH_KNOTS ( 'NONE', 3,
 ( #7882, #17657, #20496, #9574 ),
 .UNSPECIFIED., .F., .F.,
 ( 4, 4 ),
 ( 9.323472578458188095E-06, 0.0008633092105634442145 ),
 .UNSPECIFIED. ) ;
#6328 = CARTESIAN_POINT ( 'NONE',  ( 32.00490953756718682, 238.5222400402097094, -8.999999999999971578 ) ) ;
#6329 = LINE ( 'NONE', #12827, #7071 ) ;
#6330 = CIRCLE ( 'NONE', #4668, 6.500000000000000000 ) ;
#6331 = CARTESIAN_POINT ( 'NONE',  ( 225.5801007209566365, 43.01974110743358182, -13.97349461567471707 ) ) ;
#6332 = CARTESIAN_POINT ( 'NONE',  ( -27.29754541467060491, 63.83810381476320828, 5.349348394099980197 ) ) ;
#6333 = CARTESIAN_POINT ( 'NONE',  ( 80.91816734822852197, 65.18632510224837517, -25.49999999999999645 ) ) ;
#6334 = VERTEX_POINT ( 'NONE', #15406 ) ;
#6335 = CONICAL_SURFACE ( 'NONE', #1609, 4.509097725792825528, 0.5235987755983015912 ) ;
#6336 = CARTESIAN_POINT ( 'NONE',  ( -27.38439717691917608, 68.36083330498577482, 5.162430512333705757 ) ) ;
#6337 = CARTESIAN_POINT ( 'NONE',  ( 87.04593889385124328, 220.6480700052267707, 11.00000000000001066 ) ) ;
#6338 = CARTESIAN_POINT ( 'NONE',  ( 195.7881298832096775, 4.155017874419543844, -18.15810777665835474 ) ) ;
#6339 = VERTEX_POINT ( 'NONE', #20044 ) ;
#6340 = CARTESIAN_POINT ( 'NONE',  ( 58.93693122809133911, 85.22261901257984107, -10.32461968670469865 ) ) ;
#6341 = ORIENTED_EDGE ( 'NONE', *, *, #7687, .F. ) ;
#6342 = ADVANCED_FACE ( 'NONE', ( #5291 ), #16994, .T. ) ;
#6343 = ORIENTED_EDGE ( 'NONE', *, *, #9238, .F. ) ;
#6344 = CARTESIAN_POINT ( 'NONE',  ( -1.124748988296088825, 64.25000000000000000, 2.549678278787572250 ) ) ;
#6345 = DIRECTION ( 'NONE',  ( -0.8660254037844380415, -0.5000000000000014433, -0.000000000000000000 ) ) ;
#6346 = B_SPLINE_CURVE_WITH_KNOTS ( 'NONE', 3,
 ( #11654, #19797, #303, #13351 ),
 .UNSPECIFIED., .F., .F.,
 ( 4, 4 ),
 ( 2.759414894645841475E-07, 0.0006729267335475704655 ),
 .UNSPECIFIED. ) ;
#6347 = VECTOR ( 'NONE', #4577, 1000.000000000000114 ) ;
#6348 = CARTESIAN_POINT ( 'NONE',  ( 10.40000000000000036, 0.000000000000000000, 5.000000000000000888 ) ) ;
#6349 = CONTEXT_DEPENDENT_SHAPE_REPRESENTATION ( #8240, #3994 ) ;
#6350 = VECTOR ( 'NONE', #8825, 1000.000000000000114 ) ;
#6351 = CARTESIAN_POINT ( 'NONE',  ( -20.89897948556633978, 14.09941697557065332, 0.9999999999999991118 ) ) ;
#6352 = ORIENTED_EDGE ( 'NONE', *, *, #2506, .T. ) ;
#6353 = CARTESIAN_POINT ( 'NONE',  ( 205.8264633344831225, 9.596613037118636669, -14.00000000000005507 ) ) ;
#6354 = ADVANCED_FACE ( 'NONE', ( #16660 ), #545, .F. ) ;
#6355 = CARTESIAN_POINT ( 'NONE',  ( 0.000000000000000000, -1.759474945355379072, 3.047500000000001652 ) ) ;
#6356 = CARTESIAN_POINT ( 'NONE',  ( 209.6034591737553683, 30.21950843401080533, -16.37243376991346011 ) ) ;
#6357 = DIRECTION ( 'NONE',  ( 0.000000000000000000, 0.4999999999999985567, -0.8660254037844393737 ) ) ;
#6358 = CARTESIAN_POINT ( 'NONE',  ( 58.59160831385305812, 85.48790580761031777, -13.02075998189842743 ) ) ;
#6359 = CARTESIAN_POINT ( 'NONE',  ( 220.7458079535183231, 32.37244769036318104, -10.88971489487124700 ) ) ;
#6360 = CARTESIAN_POINT ( 'NONE',  ( 220.2899471553721753, 34.67552814235484959, -10.49174204642378605 ) ) ;
#6361 = DIRECTION ( 'NONE',  ( -0.5000000000000054401, 0.8660254037844354880, -0.000000000000000000 ) ) ;
#6362 = CARTESIAN_POINT ( 'NONE',  ( 217.5285743611777889, 37.94485973211421737, -14.53509620734042684 ) ) ;
#6363 = AXIS2_PLACEMENT_3D ( 'NONE', #1520, #6060, #12554 ) ;
#6364 = EDGE_LOOP ( 'NONE', ( #7027, #5350, #9184, #2797, #9709 ) ) ;
#6365 = CARTESIAN_POINT ( 'NONE',  ( 105.7973891242897650, 30.70991617951901276, -12.50000000000000000 ) ) ;
#6366 = CARTESIAN_POINT ( 'NONE',  ( 81.36345691634956268, 55.21002353147210329, -2.349880481535979282 ) ) ;
#6367 = ADVANCED_FACE ( 'NONE', ( #18244 ), #16974, .F. ) ;
#6368 = DIRECTION ( 'NONE',  ( -1.000000000000000000, 0.000000000000000000, 0.000000000000000000 ) ) ;
#6369 = CARTESIAN_POINT ( 'NONE',  ( 228.1721461148598280, 38.53018678966859056, -17.68583624946730737 ) ) ;
#6371 = VERTEX_POINT ( 'NONE', #5608 ) ;
#6370 = ORIENTED_EDGE ( 'NONE', *, *, #18466, .F. ) ;
#6372 = CARTESIAN_POINT ( 'NONE',  ( 45.00000000000000000, 5.000000000000000000, 15.00000000000000000 ) ) ;
#6373 = VERTEX_POINT ( 'NONE', #2455 ) ;
#6374 = EDGE_CURVE ( 'NONE', #9882, #2860, #3927, .T. ) ;
#6375 = CARTESIAN_POINT ( 'NONE',  ( 186.7423748293213066, 36.79335956793067197, -9.000000000000063949 ) ) ;
#6376 = EDGE_LOOP ( 'NONE', ( #19777, #20488, #7469, #10906 ) ) ;
#6377 = CARTESIAN_POINT ( 'NONE',  ( 196.8850361132133173, 4.788316981587917631, -20.67833249884100510 ) ) ;
#6378 = EDGE_CURVE ( 'NONE', #18388, #18856, #19821, .T. ) ;
#6379 = CARTESIAN_POINT ( 'NONE',  ( -28.32806265867318984, 79.99999999995431210, -2.072940693967530557 ) ) ;
#6380 = CARTESIAN_POINT ( 'NONE',  ( 85.37797649651368204, 230.0773763115391262, -26.99999999999999289 ) ) ;
#6381 = ORIENTED_EDGE ( 'NONE', *, *, #2650, .T. ) ;
#6382 = DIRECTION ( 'NONE',  ( 1.000000000000000000, 0.000000000000000000, -0.000000000000000000 ) ) ;
#6383 = B_SPLINE_CURVE_WITH_KNOTS ( 'NONE', 3,
 ( #8858, #603, #13436, #12267 ),
 .UNSPECIFIED., .F., .F.,
 ( 4, 4 ),
 ( 0.000000000000000000, 0.001416029653785006890 ),
 .UNSPECIFIED. ) ;
#6384 = EDGE_CURVE ( 'NONE', #12636, #17110, #10378, .T. ) ;
#6385 = DIRECTION ( 'NONE',  ( -0.4999999999999995004, 0.8660254037844390407, 0.000000000000000000 ) ) ;
#6386 = DIRECTION ( 'NONE',  ( -0.8660254037844360431, -0.5000000000000046629, 0.000000000000000000 ) ) ;
#6387 = ORIENTED_EDGE ( 'NONE', *, *, #11946, .T. ) ;
#6388 = CARTESIAN_POINT ( 'NONE',  ( 226.4168824216490918, 41.57039268699056578, -17.20332536629370068 ) ) ;
#6389 = DIRECTION ( 'NONE',  ( 0.5000000000000015543, -0.8660254037844377084, 0.000000000000000000 ) ) ;
#6390 = ORIENTED_EDGE ( 'NONE', *, *, #17809, .T. ) ;
#6391 = DIRECTION ( 'NONE',  ( -0.8660254037844360431, -0.5000000000000044409, 5.976026924694053325E-17 ) ) ;
#6392 = EDGE_CURVE ( 'NONE', #3291, #3585, #5397, .T. ) ;
#6393 = ORIENTED_EDGE ( 'NONE', *, *, #12803, .T. ) ;
#6394 = DIRECTION ( 'NONE',  ( 0.8660254037844369313, 0.5000000000000029976, -4.996003610813203446E-16 ) ) ;
#6395 = DIRECTION ( 'NONE',  ( 0.3430151393149145078, 0.1980398830195854720, 0.9182161068802695558 ) ) ;
#6396 = DIRECTION ( 'NONE',  ( -0.8660254037844349329, -0.5000000000000064393, 0.000000000000000000 ) ) ;
#6397 = AXIS2_PLACEMENT_3D ( 'NONE', #3565, #20304, #4093 ) ;
#6398 = EDGE_CURVE ( 'NONE', #1345, #20338, #18340, .T. ) ;
#6399 = CARTESIAN_POINT ( 'NONE',  ( 8.000000000000000000, 0.000000000000000000, 6.500000000000000000 ) ) ;
#6400 = CARTESIAN_POINT ( 'NONE',  ( -26.66531713196410891, 5.892095953840440714, -6.547001825740162317 ) ) ;
#6401 = ORIENTED_EDGE ( 'NONE', *, *, #12785, .F. ) ;
#6402 = DIRECTION ( 'NONE',  ( -0.8660254037844380415, -0.5000000000000014433, -0.000000000000000000 ) ) ;
#6403 = EDGE_CURVE ( 'NONE', #10058, #3882, #20247, .T. ) ;
#6404 = AXIS2_PLACEMENT_3D ( 'NONE', #3557, #5036, #14722 ) ;
#6405 = ADVANCED_FACE ( 'NONE', ( #15091 ), #19685, .T. ) ;
#6406 = ORIENTED_EDGE ( 'NONE', *, *, #9023, .F. ) ;
#6407 = FACE_OUTER_BOUND ( 'NONE', #19636, .T. ) ;
#6408 = CARTESIAN_POINT ( 'NONE',  ( -1.117320739478655733, 50.20017401731518447, -10.03899822371341344 ) ) ;
#6409 = DIRECTION ( 'NONE',  ( -0.5000000000000046629, 0.8660254037844360431, -0.000000000000000000 ) ) ;
#6410 = CARTESIAN_POINT ( 'NONE',  ( 85.37797649651368204, 230.0773763115391262, 1.000000000000017097 ) ) ;
#6411 = CARTESIAN_POINT ( 'NONE',  ( 96.94231704718730214, 198.6680486871722167, 11.65021776913269314 ) ) ;
#6413 = ORIENTED_EDGE ( 'NONE', *, *, #17184, .T. ) ;
#6412 = ORIENTED_EDGE ( 'NONE', *, *, #10172, .F. ) ;
#6414 = ORIENTED_EDGE ( 'NONE', *, *, #10583, .T. ) ;
#6415 = CARTESIAN_POINT ( 'NONE',  ( -15.99999999999991651, 71.61437827766162911, -4.999999999999997335 ) ) ;
#6416 = FACE_OUTER_BOUND ( 'NONE', #9423, .T. ) ;
#6417 = EDGE_CURVE ( 'NONE', #13052, #566, #10398, .T. ) ;
#6418 = CARTESIAN_POINT ( 'NONE',  ( -10.55030972131536338, 80.00000000004204992, -11.26030642047042996 ) ) ;
#6419 = ORIENTED_EDGE ( 'NONE', *, *, #10793, .T. ) ;
#6420 = VERTEX_POINT ( 'NONE', #3822 ) ;
#6421 = FACE_OUTER_BOUND ( 'NONE', #17690, .T. ) ;
#6422 = DIRECTION ( 'NONE',  ( 0.000000000000000000, 0.000000000000000000, 1.000000000000000000 ) ) ;
#6423 = PRESENTATION_LAYER_ASSIGNMENT (  '', '', ( #4079 ) ) ;
#6424 = CARTESIAN_POINT ( 'NONE',  ( -12.09679518933233311, 61.49126500257621331, -3.129598480498282598 ) ) ;
#6425 = VERTEX_POINT ( 'NONE', #6892 ) ;
#6426 = AXIS2_PLACEMENT_3D ( 'NONE', #6594, #1745, #12885 ) ;
#6427 = ORIENTED_EDGE ( 'NONE', *, *, #12987, .T. ) ;
#6428 = DIRECTION ( 'NONE',  ( 0.000000000000000000, -0.8532072764867938419, -0.5215719924899993032 ) ) ;
#6429 = EDGE_CURVE ( 'NONE', #3253, #16503, #18354, .T. ) ;
#6430 = AXIS2_PLACEMENT_3D ( 'NONE', #16430, #14860, #13148 ) ;
#6431 = LINE ( 'NONE', #11430, #15561 ) ;
#6432 = VECTOR ( 'NONE', #17937, 1000.000000000000114 ) ;
#6433 = CARTESIAN_POINT ( 'NONE',  ( 209.8909370991932235, 2.556737970610013733, -14.00000000000005507 ) ) ;
#6434 = CARTESIAN_POINT ( 'NONE',  ( -28.99999999999999289, 0.000000000000000000, -15.00000000000000000 ) ) ;
#6435 = CARTESIAN_POINT ( 'NONE',  ( 22.00490953756706958, 255.8427481158984165, 1.000000000000018208 ) ) ;
#6436 = CIRCLE ( 'NONE', #3072, 3.902363844300875240 ) ;
#6437 = PLANE ( 'NONE',  #15504 ) ;
#6438 = VECTOR ( 'NONE', #16718, 1000.000000000000227 ) ;
#6439 = CARTESIAN_POINT ( 'NONE',  ( 99.99529059433426426, 150.7594456239217777, 1.000000000000006883 ) ) ;
#6440 = ORIENTED_EDGE ( 'NONE', *, *, #2828, .T. ) ;
#6441 = CARTESIAN_POINT ( 'NONE',  ( 62.46278923780241144, 78.25414160106842587, -9.766604451679548049 ) ) ;
#6442 = CIRCLE ( 'NONE', #1731, 1.500000000000001332 ) ;
#6443 = ORIENTED_EDGE ( 'NONE', *, *, #14431, .T. ) ;
#6444 = VERTEX_POINT ( 'NONE', #5507 ) ;
#6445 = CARTESIAN_POINT ( 'NONE',  ( 5.000000000000000000, 4.685197434473812983, -6.938893903907228378E-15 ) ) ;
#6446 = AXIS2_PLACEMENT_3D ( 'NONE', #18293, #3556, #10001 ) ;
#6447 = VECTOR ( 'NONE', #189, 1000.000000000000227 ) ;
#6448 = CARTESIAN_POINT ( 'NONE',  ( -14.37945692259737207, 10.36644441490629909, 12.39552528635021034 ) ) ;
#6449 = VERTEX_POINT ( 'NONE', #8697 ) ;
#6450 = CARTESIAN_POINT ( 'NONE',  ( -18.33199948130959100, 79.99972521406444059, -12.39529528716347428 ) ) ;
#6451 = AXIS2_PLACEMENT_3D ( 'NONE', #3435, #256, #17761 ) ;
#6452 = LINE ( 'NONE', #17821, #3847 ) ;
#6453 = VERTEX_POINT ( 'NONE', #15196 ) ;
#6454 = FACE_OUTER_BOUND ( 'NONE', #659, .T. ) ;
#6455 = CARTESIAN_POINT ( 'NONE',  ( 211.4194833127196489, 27.45139579749023540, -14.00000000000004974 ) ) ;
#6456 = PLANE ( 'NONE',  #8487 ) ;
#6457 = DIRECTION ( 'NONE',  ( 0.2483788854153066994, 0.1434016163555488221, 0.9579895123154877901 ) ) ;
#6458 = CARTESIAN_POINT ( 'NONE',  ( 59.65554463217813463, 240.6299351947967011, -13.99999999999998046 ) ) ;
#6459 = CARTESIAN_POINT ( 'NONE',  ( 44.00000000000000000, 0.000000000000000000, -15.00000000000000355 ) ) ;
#6460 = AXIS2_PLACEMENT_3D ( 'NONE', #7685, #921, #4204 ) ;
#6461 = CARTESIAN_POINT ( 'NONE',  ( 203.7294658059541064, 23.22871929987706707, -14.00000000000005507 ) ) ;
#6462 = CARTESIAN_POINT ( 'NONE',  ( 30.92607121268107306, 174.3908428320655446, 11.00000000000001243 ) ) ;
#6463 = EDGE_LOOP ( 'NONE', ( #5968, #9389, #2535, #17994, #13596, #19936 ) ) ;
#6464 = ORIENTED_EDGE ( 'NONE', *, *, #16876, .T. ) ;
#6465 = AXIS2_PLACEMENT_3D ( 'NONE', #20706, #5958, #15747 ) ;
#6466 = B_SPLINE_CURVE_WITH_KNOTS ( 'NONE', 3,
 ( #7701, #12805, #1356, #6411, #3352, #3151, #16095, #11311, #1562, #3246, #12702, #14307, #16195, #20741, #19060, #1667, #19161, #1460 ),
 .UNSPECIFIED., .F., .F.,
 ( 4, 2, 2, 2, 2, 2, 2, 2, 4 ),
 ( 0.003919784392900028426, 0.004409243773870153045, 0.004898703154840278531, 0.005388162535810403150, 0.005877621916780527769, 0.006367081297750653256, 0.006856540678720777875, 0.007346000059690903361, 0.007835459440661027980 ),
 .UNSPECIFIED. ) ;
#6467 = FACE_OUTER_BOUND ( 'NONE', #11632, .T. ) ;
#6468 = DIRECTION ( 'NONE',  ( 0.000000000000000000, 0.000000000000000000, -1.000000000000000000 ) ) ;
#6469 = VECTOR ( 'NONE', #6171, 1000.000000000000227 ) ;
#6470 = ADVANCED_FACE ( 'NONE', ( #761 ), #19042, .T. ) ;
#6471 = CARTESIAN_POINT ( 'NONE',  ( 199.2144802262915846, 21.04890371929339921, -14.00000000000005507 ) ) ;
#6472 = DIRECTION ( 'NONE',  ( 0.4758887346169383692, 0.2747544890354036706, -0.8354878114129394850 ) ) ;
#6473 = CONICAL_SURFACE ( 'NONE', #11918, 13.07248899748297433, 0.6693469023067423196 ) ;
#6475 = ORIENTED_EDGE ( 'NONE', *, *, #9374, .F. ) ;
#6474 = EDGE_LOOP ( 'NONE', ( #587, #1904, #13724, #14859, #9395 ) ) ;
#6476 = CARTESIAN_POINT ( 'NONE',  ( 214.2619155600624481, 14.99787291208556539, -20.59651891138172530 ) ) ;
#6477 = ORIENTED_EDGE ( 'NONE', *, *, #1068, .T. ) ;
#6478 = CIRCLE ( 'NONE', #10543, 4.057500000000000107 ) ;
#6479 = CARTESIAN_POINT ( 'NONE',  ( -32.41958609996412122, 70.63162242946638969, 1.437809060325973221 ) ) ;
#6480 = ORIENTED_EDGE ( 'NONE', *, *, #15516, .T. ) ;
#6481 = CARTESIAN_POINT ( 'NONE',  ( 174.9952905943348469, 20.85563505625644609, -14.00000000000000533 ) ) ;
#6482 = CARTESIAN_POINT ( 'NONE',  ( -29.47154141322603138, 77.37584602520398391, -3.922623763563328314 ) ) ;
#6483 = AXIS2_PLACEMENT_3D ( 'NONE', #9972, #8822, #7015 ) ;
#6484 = CARTESIAN_POINT ( 'NONE',  ( 208.4761278624580711, 5.007259451653140125, -14.00000000000005507 ) ) ;
#6485 = ADVANCED_FACE ( 'NONE', ( #13591 ), #17083, .F. ) ;
#6486 = CONICAL_SURFACE ( 'NONE', #15670, 4.389613146203297234, 1.047197551196619614 ) ;
#6487 = B_SPLINE_CURVE_WITH_KNOTS ( 'NONE', 3,
 ( #2525, #8771, #15372, #10563 ),
 .UNSPECIFIED., .F., .F.,
 ( 4, 4 ),
 ( 2.740756717971691198E-07, 0.0006729248677300605315 ),
 .UNSPECIFIED. ) ;
#6488 = DIRECTION ( 'NONE',  ( 0.2597919750177186682, -0.4499729001293500397, -0.8544194045464880150 ) ) ;
#6489 = CARTESIAN_POINT ( 'NONE',  ( 60.01640235382483013, 75.53995351896973887, -4.869773649086239331 ) ) ;
#6490 = FACE_OUTER_BOUND ( 'NONE', #12913, .T. ) ;
#6491 = ORIENTED_EDGE ( 'NONE', *, *, #1006, .F. ) ;
#6492 = ADVANCED_FACE ( 'NONE', ( #18565 ), #8481, .F. ) ;
#6493 = CARTESIAN_POINT ( 'NONE',  ( 222.1527769467159601, 32.06686066723883499, -13.49489896056993743 ) ) ;
#6494 = ADVANCED_FACE ( 'NONE', ( #1075 ), #17395, .F. ) ;
#6495 = ORIENTED_EDGE ( 'NONE', *, *, #17003, .T. ) ;
#6496 = CARTESIAN_POINT ( 'NONE',  ( 209.9464292287906630, 27.24499736481567069, -15.43274561385901400 ) ) ;
#6497 = CONICAL_SURFACE ( 'NONE', #19701, 4.999999999999944933, 1.566852922939436121 ) ;
#6498 = VECTOR ( 'NONE', #5881, 1000.000000000000114 ) ;
#6499 = EDGE_LOOP ( 'NONE', ( #14458, #410, #15745, #19321, #8326, #17712, #17113, #4867, #5569, #20005, #9614, #7570 ) ) ;
#6500 = CARTESIAN_POINT ( 'NONE',  ( 5.000000000000004441, -4.685197434473809430, 6.071532165918824830E-15 ) ) ;
#6501 = CARTESIAN_POINT ( 'NONE',  ( 0.000000000000000000, -10.00000000000000000, 0.000000000000000000 ) ) ;
#6502 = CARTESIAN_POINT ( 'NONE',  ( 220.0479314030272064, 35.09471172164835906, -17.56803216753791475 ) ) ;
#6503 = LINE ( 'NONE', #13207, #9992 ) ;
#6504 = CARTESIAN_POINT ( 'NONE',  ( -26.00000000000000000, 5.000000000000001776, -7.500000000000000000 ) ) ;
#6505 = LINE ( 'NONE', #19657, #13019 ) ;
#6506 = ORIENTED_EDGE ( 'NONE', *, *, #315, .F. ) ;
#6507 = CARTESIAN_POINT ( 'NONE',  ( 26.00000000000000355, 0.000000000000000000, 0.000000000000000000 ) ) ;
#6508 = DIRECTION ( 'NONE',  ( 0.8660254037844355990, 0.5000000000000054401, 0.000000000000000000 ) ) ;
#6509 = CIRCLE ( 'NONE', #9226, 17.50000000000000000 ) ;
#6510 = EDGE_CURVE ( 'NONE', #11555, #2596, #12726, .T. ) ;
#6511 = ORIENTED_EDGE ( 'NONE', *, *, #16391, .T. ) ;
#6512 = LINE ( 'NONE', #6616, #13600 ) ;
#6513 = CARTESIAN_POINT ( 'NONE',  ( -12.60528683216188739, 45.48061573273304958, -12.04982389388483632 ) ) ;
#6514 = CARTESIAN_POINT ( 'NONE',  ( 1.237363539717748262, 77.39914922625320060, -4.045904646045205055 ) ) ;
#6515 = ADVANCED_FACE ( 'NONE', ( #4563 ), #7410, .T. ) ;
#6516 = PLANE ( 'NONE',  #8099 ) ;
#6517 = CARTESIAN_POINT ( 'NONE',  ( -24.71655914096720608, 44.99675394863319866, -8.967748501840956621 ) ) ;
#6519 = ORIENTED_EDGE ( 'NONE', *, *, #11860, .F. ) ;
#6518 = ORIENTED_EDGE ( 'NONE', *, *, #2767, .T. ) ;
#6520 = ORIENTED_EDGE ( 'NONE', *, *, #5993, .T. ) ;
#6521 = DIRECTION ( 'NONE',  ( 0.5000000000000041078, -0.8660254037844363761, 0.000000000000000000 ) ) ;
#6522 = PLANE ( 'NONE',  #7127 ) ;
#6523 = EDGE_CURVE ( 'NONE', #15273, #20835, #12195, .T. ) ;
#6524 = ORIENTED_EDGE ( 'NONE', *, *, #14083, .T. ) ;
#6525 = CARTESIAN_POINT ( 'NONE',  ( -19.20871456446631598, 60.00315144574870629, -3.836613224171040670 ) ) ;
#6526 = FACE_OUTER_BOUND ( 'NONE', #6139, .T. ) ;
#6527 = CARTESIAN_POINT ( 'NONE',  ( -31.83568508345510750, 63.85501752543220988, 2.461464410061926955 ) ) ;
#6528 = CARTESIAN_POINT ( 'NONE',  ( 37.00490953756721524, 229.8619860023653985, 26.00000000000001776 ) ) ;
#6529 = CONICAL_SURFACE ( 'NONE', #472, 13.07248899748297433, 0.6693469023067423196 ) ;
#6530 = VERTEX_POINT ( 'NONE', #20662 ) ;
#6531 = ADVANCED_FACE ( 'NONE', ( #9420 ), #1385, .T. ) ;
#6532 = EDGE_LOOP ( 'NONE', ( #11117, #8649, #7240, #11910 ) ) ;
#6533 = LINE ( 'NONE', #11647, #14153 ) ;
#6534 = FACE_OUTER_BOUND ( 'NONE', #7907, .T. ) ;
#6535 = ADVANCED_FACE ( 'NONE', ( #14016 ), #4462, .F. ) ;
#6536 = DIRECTION ( 'NONE',  ( 0.5000000000000058842, -0.8660254037844351549, 0.000000000000000000 ) ) ;
#6537 = DIRECTION ( 'NONE',  ( -0.8660254037844378194, -0.5000000000000013323, -0.000000000000000000 ) ) ;
#6538 = CARTESIAN_POINT ( 'NONE',  ( 80.22377123718597147, 65.83756043191739593, -25.47379904941673345 ) ) ;
#6539 = VECTOR ( 'NONE', #4672, 1000.000000000000227 ) ;
#6540 = VECTOR ( 'NONE', #9950, 1000.000000000000000 ) ;
#6541 = ORIENTED_EDGE ( 'NONE', *, *, #16106, .F. ) ;
#6542 = CARTESIAN_POINT ( 'NONE',  ( 32.36389338619004263, 157.9004617752989930, -29.00000000000000000 ) ) ;
#6543 = DIRECTION ( 'NONE',  ( 0.000000000000000000, 0.4999999999999985012, -0.8660254037844394848 ) ) ;
#6544 = ORIENTED_EDGE ( 'NONE', *, *, #17260, .T. ) ;
#6545 = ORIENTED_EDGE ( 'NONE', *, *, #20760, .T. ) ;
#6546 = EDGE_CURVE ( 'NONE', #8080, #4182, #10805, .T. ) ;
#6547 = CARTESIAN_POINT ( 'NONE',  ( 63.96297526125024291, 77.36452158080264496, -7.208114797878260482 ) ) ;
#6548 = ORIENTED_EDGE ( 'NONE', *, *, #18030, .F. ) ;
#6549 = DIRECTION ( 'NONE',  ( 0.000000000000000000, -1.000000000000000000, 0.000000000000000000 ) ) ;
#6550 = ADVANCED_FACE ( 'NONE', ( #9310 ), #15815, .F. ) ;
#6551 = EDGE_CURVE ( 'NONE', #8176, #5372, #14659, .T. ) ;
#6552 = ORIENTED_EDGE ( 'NONE', *, *, #8768, .T. ) ;
#6553 = CARTESIAN_POINT ( 'NONE',  ( 173.9132435853527454, 54.87193107572242212, -14.00000000000002842 ) ) ;
#6554 = VECTOR ( 'NONE', #6019, 1000.000000000000227 ) ;
#6555 = EDGE_CURVE ( 'NONE', #7692, #6339, #15606, .T. ) ;
#6556 = LINE ( 'NONE', #20874, #11300 ) ;
#6557 = ORIENTED_EDGE ( 'NONE', *, *, #8622, .F. ) ;
#6558 = CYLINDRICAL_SURFACE ( 'NONE', #7051, 5.000000000000036415 ) ;
#6559 = DIRECTION ( 'NONE',  ( -0.5000000000000045519, 0.8660254037844360431, 0.000000000000000000 ) ) ;
#6560 = CARTESIAN_POINT ( 'NONE',  ( -0.1517743604773433008, 63.45732323195518632, 2.441554792792626660 ) ) ;
#6561 = EDGE_CURVE ( 'NONE', #14336, #12562, #14127, .T. ) ;
#6563 = CYLINDRICAL_SURFACE ( 'NONE', #15784, 13.50000000000000711 ) ;
#6562 = B_SPLINE_CURVE_WITH_KNOTS ( 'NONE', 3,
 ( #9946, #643, #14872, #6771 ),
 .UNSPECIFIED., .F., .F.,
 ( 4, 4 ),
 ( 4.013812776618870414E-06, 0.0004560670545565227068 ),
 .UNSPECIFIED. ) ;
#6564 = DIRECTION ( 'NONE',  ( -0.8660254037844361541, -0.5000000000000044409, 5.976026924694052093E-17 ) ) ;
#6565 = LINE ( 'NONE', #13481, #14934 ) ;
#6566 = DIRECTION ( 'NONE',  ( 0.000000000000000000, 0.000000000000000000, -1.000000000000000000 ) ) ;
#6567 = FACE_OUTER_BOUND ( 'NONE', #19026, .T. ) ;
#6568 = ORIENTED_EDGE ( 'NONE', *, *, #5122, .F. ) ;
#6569 = CIRCLE ( 'NONE', #18444, 3.902363844300875240 ) ;
#6570 = EDGE_LOOP ( 'NONE', ( #9153, #3130, #8764, #16268, #15703 ) ) ;
#6571 = EDGE_CURVE ( 'NONE', #13886, #918, #12226, .T. ) ;
#6572 = CARTESIAN_POINT ( 'NONE',  ( 184.9952905943349606, 3.535126980567727450, -29.00000000000001066 ) ) ;
#6573 = CARTESIAN_POINT ( 'NONE',  ( 75.24208973902655373, 72.42691426209449901, -0.2122651547815246897 ) ) ;
#6574 = CARTESIAN_POINT ( 'NONE',  ( -14.60189797479694818, 71.38521106151608819, -4.803508630518933842 ) ) ;
#6575 = CARTESIAN_POINT ( 'NONE',  ( 76.31847140867067480, 53.71537708853300330, -19.03182057956520978 ) ) ;
#6577 = ORIENTED_EDGE ( 'NONE', *, *, #15917, .F. ) ;
#6576 = ORIENTED_EDGE ( 'NONE', *, *, #10362, .F. ) ;
#6578 = VERTEX_POINT ( 'NONE', #7522 ) ;
#6579 = DIRECTION ( 'NONE',  ( 0.000000000000000000, 0.000000000000000000, -1.000000000000000000 ) ) ;
#6580 = ORIENTED_EDGE ( 'NONE', *, *, #2816, .T. ) ;
#6581 = EDGE_CURVE ( 'NONE', #3518, #1818, #18881, .T. ) ;
#6582 = CARTESIAN_POINT ( 'NONE',  ( -33.48481952675158624, 76.25000000000001421, -2.578432583507804132 ) ) ;
#6583 = ORIENTED_EDGE ( 'NONE', *, *, #18766, .T. ) ;
#6584 = SURFACE_SIDE_STYLE ('',( #13083 ) ) ;
#6585 = CARTESIAN_POINT ( 'NONE',  ( -29.45159263616708500, 77.71408077849254425, -4.406821185033810373 ) ) ;
#6586 = CARTESIAN_POINT ( 'NONE',  ( 198.4292936038012840, 5.502877782304041787, -22.95081059697375991 ) ) ;
#6587 = EDGE_CURVE ( 'NONE', #14688, #4229, #6605, .T. ) ;
#6588 = CIRCLE ( 'NONE', #19472, 0.9999999999999917843 ) ;
#6589 = FACE_OUTER_BOUND ( 'NONE', #13633, .T. ) ;
#6590 = CARTESIAN_POINT ( 'NONE',  ( 54.32368702807821137, 77.96689879364747355, -13.45758936859397004 ) ) ;
#6591 = CARTESIAN_POINT ( 'NONE',  ( 200.1605181682011221, -0.5665801344454006738, -7.448751785191272567 ) ) ;
#6592 = ORIENTED_EDGE ( 'NONE', *, *, #8222, .T. ) ;
#6593 = CARTESIAN_POINT ( 'NONE',  ( 226.6211368133091923, 39.11482588413117867, -14.00000000000005507 ) ) ;
#6594 = CARTESIAN_POINT ( 'NONE',  ( 217.1880081454256981, 38.53473772113837725, -13.42327856638893913 ) ) ;
#6595 = ORIENTED_EDGE ( 'NONE', *, *, #18053, .F. ) ;
#6596 = AXIS2_PLACEMENT_3D ( 'NONE', #16514, #13341, #19789 ) ;
#6597 = FACE_OUTER_BOUND ( 'NONE', #1514, .T. ) ;
#6598 = ADVANCED_FACE ( 'NONE', ( #1180 ), #6032, .T. ) ;
#6599 = VERTEX_POINT ( 'NONE', #8643 ) ;
#6600 = VECTOR ( 'NONE', #6559, 1000.000000000000114 ) ;
#6601 = CARTESIAN_POINT ( 'NONE',  ( 211.1008594470266360, 27.84852471586090772, -12.46092303668267398 ) ) ;
#6602 = DIRECTION ( 'NONE',  ( 0.000000000000000000, 0.000000000000000000, -1.000000000000000000 ) ) ;
#6603 = VECTOR ( 'NONE', #11147, 1000.000000000000000 ) ;
#6604 = DIRECTION ( 'NONE',  ( 0.000000000000000000, 0.000000000000000000, 1.000000000000000000 ) ) ;
#6605 = B_SPLINE_CURVE_WITH_KNOTS ( 'NONE', 3,
 ( #9212, #15717, #12628, #14231 ),
 .UNSPECIFIED., .F., .F.,
 ( 4, 4 ),
 ( 1.635950431741829803E-05, 0.0005822857266139719930 ),
 .UNSPECIFIED. ) ;
#6606 = DIRECTION ( 'NONE',  ( 0.5000000000000057732, -0.8660254037844353769, 0.000000000000000000 ) ) ;
#6607 = DIRECTION ( 'NONE',  ( -0.8660254037844375974, -0.5000000000000018874, 0.000000000000000000 ) ) ;
#6608 = DIRECTION ( 'NONE',  ( 0.5000000000000054401, -0.8660254037844354880, 0.000000000000000000 ) ) ;
#6609 = VERTEX_POINT ( 'NONE', #11628 ) ;
#6610 = EDGE_CURVE ( 'NONE', #14942, #9307, #18090, .T. ) ;
#6611 = CARTESIAN_POINT ( 'NONE',  ( 78.29269775295045974, 67.14660545764391486, -25.32607527901491196 ) ) ;
#6612 = VECTOR ( 'NONE', #9791, 1000.000000000000000 ) ;
#6613 = DIRECTION ( 'NONE',  ( 0.000000000000000000, -0.4999999999999985567, 0.8660254037844393737 ) ) ;
#6614 = ORIENTED_EDGE ( 'NONE', *, *, #8251, .T. ) ;
#6615 = AXIS2_PLACEMENT_3D ( 'NONE', #3085, #14446, #10813 ) ;
#6616 = CARTESIAN_POINT ( 'NONE',  ( 85.37797649651368204, 230.0773763115391262, -0.9999999999999826805 ) ) ;
#6617 = CARTESIAN_POINT ( 'NONE',  ( -4.201979992901475391, 56.88514657979481370, 4.132832673961413406 ) ) ;
#6618 = CARTESIAN_POINT ( 'NONE',  ( -15.99999999999999289, 80.00000000000000000, 12.50000000000000000 ) ) ;
#6619 = AXIS2_PLACEMENT_3D ( 'NONE', #11209, #12911, #19365 ) ;
#6620 = CARTESIAN_POINT ( 'NONE',  ( 115.7566812678108050, 36.45991617951907671, -12.49999999999999822 ) ) ;
#6621 = CARTESIAN_POINT ( 'NONE',  ( 43.00000000000000000, 0.000000000000000000, 0.000000000000000000 ) ) ;
#6622 = ORIENTED_EDGE ( 'NONE', *, *, #17520, .F. ) ;
#6623 = ORIENTED_EDGE ( 'NONE', *, *, #4208, .F. ) ;
#6624 = ORIENTED_EDGE ( 'NONE', *, *, #14833, .F. ) ;
#6625 = CARTESIAN_POINT ( 'NONE',  ( 226.0260823154428067, 42.24727832654306070, -16.48323849494058635 ) ) ;
#6626 = DIRECTION ( 'NONE',  ( 0.000000000000000000, 0.000000000000000000, -1.000000000000000000 ) ) ;
#6627 = ORIENTED_EDGE ( 'NONE', *, *, #19689, .F. ) ;
#6628 = VERTEX_POINT ( 'NONE', #13429 ) ;
#6629 = CARTESIAN_POINT ( 'NONE',  ( -18.90941040546627860, 59.62118480013949551, -4.068652614656587119 ) ) ;
#6630 = DIRECTION ( 'NONE',  ( -0.8660254037844375974, -0.5000000000000019984, 0.000000000000000000 ) ) ;
#6631 = LINE ( 'NONE', #13125, #15293 ) ;
#6632 = CIRCLE ( 'NONE', #18504, 5.999999999999989342 ) ;
#6633 = CARTESIAN_POINT ( 'NONE',  ( -15.64137421610944578, 58.39658375749213803, -4.990290896351837091 ) ) ;
#6634 = EDGE_LOOP ( 'NONE', ( #7373, #5450, #18106, #86 ) ) ;
#6635 = ORIENTED_EDGE ( 'NONE', *, *, #10708, .T. ) ;
#6636 = AXIS2_PLACEMENT_3D ( 'NONE', #8437, #11527, #1887 ) ;
#6637 = CARTESIAN_POINT ( 'NONE',  ( 81.06711713768373784, 65.00000000000000000, 0.4999999999999962252 ) ) ;
#6638 = ADVANCED_FACE ( 'NONE', ( #5141 ), #11731, .F. ) ;
#6639 = EDGE_CURVE ( 'NONE', #8949, #7633, #19874, .T. ) ;
#6640 = DIRECTION ( 'NONE',  ( -0.8660254037844361541, -0.5000000000000045519, 5.976026924694054558E-17 ) ) ;
#6641 = DIRECTION ( 'NONE',  ( -0.8601696498176567562, -0.4966191788709768962, -0.1160929141252230179 ) ) ;
#6642 = CARTESIAN_POINT ( 'NONE',  ( -27.29940250357268283, 45.63043474242538622, -5.355865623545788878 ) ) ;
#6643 = CARTESIAN_POINT ( 'NONE',  ( 205.0662616026534693, 10.91332106064940888, -14.00000000000005507 ) ) ;
#6644 = PLANE ( 'NONE',  #13908 ) ;
#6645 = CARTESIAN_POINT ( 'NONE',  ( 220.2180084519553134, 35.41797800104779270, -14.00000000000005507 ) ) ;
#6646 = EDGE_CURVE ( 'NONE', #1746, #20139, #11431, .T. ) ;
#6647 = VECTOR ( 'NONE', #15232, 1000.000000000000227 ) ;
#6648 = VERTEX_POINT ( 'NONE', #18191 ) ;
#6649 = B_SPLINE_CURVE_WITH_KNOTS ( 'NONE', 3,
 ( #15896, #2753, #18864, #4337, #12612, #2648, #9194, #9091, #7920, #12713, #9294, #15700, #14419, #1166, #4649, #4545, #12822, #3057, #14105, #7614, #6012, #12502, #18963, #4441 ),
 .UNSPECIFIED., .F., .F.,
 ( 4, 2, 2, 2, 2, 2, 2, 2, 2, 2, 2, 4 ),
 ( 0.000000000000000000, 0.002039071642891474370, 0.003058607464337211555, 0.004078143285782949608, 0.006117214928674423111, 0.007136750750120161163, 0.008156286571565897481, 0.009175822393011635533, 0.01019535821445737185, 0.01223442985734884796, 0.01427350150024032753, 0.01631257314313180537 ),
 .UNSPECIFIED. ) ;
#6650 = CARTESIAN_POINT ( 'NONE',  ( 62.58256123368390433, 78.18905788646169697, -12.55308404828634039 ) ) ;
#6651 = ORIENTED_EDGE ( 'NONE', *, *, #7317, .F. ) ;
#6652 = DIRECTION ( 'NONE',  ( -0.5000000000000045519, 0.8660254037844359321, 0.000000000000000000 ) ) ;
#6653 = CARTESIAN_POINT ( 'NONE',  ( 62.00490953756744972, 186.5607158131434744, 26.00000000000001776 ) ) ;
#6654 = EDGE_CURVE ( 'NONE', #17576, #14829, #17711, .T. ) ;
#6655 = ORIENTED_EDGE ( 'NONE', *, *, #2804, .T. ) ;
#6656 = CARTESIAN_POINT ( 'NONE',  ( 196.7640869814540565, 9.019494789394645551, -5.407152407593843968 ) ) ;
#6657 = EDGE_LOOP ( 'NONE', ( #3854, #11901, #8984, #12141 ) ) ;
#6658 = EDGE_CURVE ( 'NONE', #9199, #11172, #12834, .T. ) ;
#6659 = DIRECTION ( 'NONE',  ( 0.000000000000000000, -1.000000000000000000, 0.000000000000000000 ) ) ;
#6660 = ORIENTED_EDGE ( 'NONE', *, *, #4043, .T. ) ;
#6661 = CIRCLE ( 'NONE', #17174, 3.902363844300875240 ) ;
#6662 = CARTESIAN_POINT ( 'NONE',  ( 213.0703269268611848, 13.95588231258707701, -22.95081059697398373 ) ) ;
#6663 = CARTESIAN_POINT ( 'NONE',  ( 218.7490010597510945, 37.34452507169554991, -11.35524774226742650 ) ) ;
#6664 = CONICAL_SURFACE ( 'NONE', #3297, 1.499999999999990896, 0.8526294284052392536 ) ;
#6665 = LINE ( 'NONE', #16143, #15111 ) ;
#6666 = FACE_OUTER_BOUND ( 'NONE', #5854, .T. ) ;
#6667 = ADVANCED_FACE ( 'NONE', ( #9629 ), #1591, .T. ) ;
#6668 = ORIENTED_EDGE ( 'NONE', *, *, #11825, .T. ) ;
#6669 = LINE ( 'NONE', #16442, #12895 ) ;
#6670 = DIRECTION ( 'NONE',  ( -0.8660254037844354880, -0.5000000000000055511, 0.000000000000000000 ) ) ;
#6671 = DIRECTION ( 'NONE',  ( -1.000000000000000000, 0.000000000000000000, 0.000000000000000000 ) ) ;
#6672 = EDGE_CURVE ( 'NONE', #15862, #20176, #10167, .T. ) ;
#6673 = ORIENTED_EDGE ( 'NONE', *, *, #16258, .F. ) ;
#6674 = LINE ( 'NONE', #13169, #1397 ) ;
#6675 = CARTESIAN_POINT ( 'NONE',  ( 82.90799867058008488, 61.47212875548994049, 0.2523705075321406865 ) ) ;
#6676 = AXIS2_PLACEMENT_3D ( 'NONE', #19329, #9569, #14478 ) ;
#6677 = DIRECTION ( 'NONE',  ( -1.000000000000000000, -0.000000000000000000, -0.000000000000000000 ) ) ;
#6678 = CARTESIAN_POINT ( 'NONE',  ( 79.43779261569734729, 49.71110166847581979, -14.71424312708910698 ) ) ;
#6679 = EDGE_CURVE ( 'NONE', #7529, #1461, #275, .T. ) ;
#6680 = VECTOR ( 'NONE', #17383, 1000.000000000000227 ) ;
#6682 = ORIENTED_EDGE ( 'NONE', *, *, #13159, .T. ) ;
#6681 = ORIENTED_EDGE ( 'NONE', *, *, #2139, .T. ) ;
#6683 = ORIENTED_EDGE ( 'NONE', *, *, #4219, .F. ) ;
#6684 = VERTEX_POINT ( 'NONE', #8541 ) ;
#6685 = DIRECTION ( 'NONE',  ( -0.8660254037844357100, -0.5000000000000049960, 0.000000000000000000 ) ) ;
#6686 = ORIENTED_EDGE ( 'NONE', *, *, #13188, .T. ) ;
#6687 = CARTESIAN_POINT ( 'NONE',  ( 220.2180084519553134, 35.41797800104779270, -14.00000000000005507 ) ) ;
#6688 = ADVANCED_FACE ( 'NONE', ( #13531 ), #2757, .T. ) ;
#6689 = CARTESIAN_POINT ( 'NONE',  ( 219.1832987529824663, 36.56227459534655111, -17.22762539913929558 ) ) ;
#6690 = DIRECTION ( 'NONE',  ( -1.000000000000000000, -0.000000000000000000, -0.000000000000000000 ) ) ;
#6691 = ORIENTED_EDGE ( 'NONE', *, *, #2234, .T. ) ;
#6692 = AXIS2_PLACEMENT_3D ( 'NONE', #6481, #12982, #17855 ) ;
#6693 = CARTESIAN_POINT ( 'NONE',  ( 196.7929107858857094, 4.381089041447214782, -20.84195174293567376 ) ) ;
#6694 = AXIS2_PLACEMENT_3D ( 'NONE', #5406, #15313, #15414 ) ;
#6695 = CARTESIAN_POINT ( 'NONE',  ( 54.38430900759308884, 77.94115371992377561, -11.24098572673000795 ) ) ;
#6696 = DIRECTION ( 'NONE',  ( -0.7235536692358652822, -0.4177439057064742944, -0.5495089780708012350 ) ) ;
#6697 = ORIENTED_EDGE ( 'NONE', *, *, #2928, .F. ) ;
#6698 = CARTESIAN_POINT ( 'NONE',  ( 220.6654489287540741, 32.51163360410156145, -16.29291827778590829 ) ) ;
#6699 = FACE_OUTER_BOUND ( 'NONE', #10330, .T. ) ;
#6700 = ORIENTED_EDGE ( 'NONE', *, *, #20901, .T. ) ;
#6701 = CARTESIAN_POINT ( 'NONE',  ( 200.2378745322256464, -0.5219184168523266498, -7.515250618841284869 ) ) ;
#6702 = ORIENTED_EDGE ( 'NONE', *, *, #723, .F. ) ;
#6703 = B_SPLINE_CURVE_WITH_KNOTS ( 'NONE', 3,
 ( #15814, #5823, #1286, #7731 ),
 .UNSPECIFIED., .F., .F.,
 ( 4, 4 ),
 ( 2.987124294343826120E-07, 0.0004523519542092925604 ),
 .UNSPECIFIED. ) ;
#6704 = AXIS2_PLACEMENT_3D ( 'NONE', #15947, #4796, #4594 ) ;
#6705 = CARTESIAN_POINT ( 'NONE',  ( 211.4194833127196205, 27.45139579749023540, -13.83454964029852086 ) ) ;
#6706 = FACE_OUTER_BOUND ( 'NONE', #8750, .T. ) ;
#6707 = DIRECTION ( 'NONE',  ( -0.8660254037844355990, -0.5000000000000055511, 0.000000000000000000 ) ) ;
#6708 = CARTESIAN_POINT ( 'NONE',  ( 169.8972143829816730, 23.68576207517868326, -14.00000000000007461 ) ) ;
#6709 = CARTESIAN_POINT ( 'NONE',  ( -27.12730151730438521, 6.201679376448834269, -5.736216294243367209 ) ) ;
#6710 = SHAPE_REPRESENTATION_RELATIONSHIP ( 'NONE' , 'NONE' ,  #3951, #15173 ) ;
#6711 = LINE ( 'NONE', #6125, #18428 ) ;
#6712 = ORIENTED_EDGE ( 'NONE', *, *, #3426, .T. ) ;
#6713 = CARTESIAN_POINT ( 'NONE',  ( 79.89995321854216570, 66.11592257250090654, -25.45829505270997117 ) ) ;
#6714 = CARTESIAN_POINT ( 'NONE',  ( -4.701390418375632763, 64.25000000000000000, 5.347094680480811490 ) ) ;
#6715 = VECTOR ( 'NONE', #16730, 1000.000000000000114 ) ;
#6716 = VERTEX_POINT ( 'NONE', #7048 ) ;
#6717 = CARTESIAN_POINT ( 'NONE',  ( 5.000000000000000000, -4.685197434473809430, 6.071532165918824830E-15 ) ) ;
#6718 = CARTESIAN_POINT ( 'NONE',  ( -3.770603668498050176, 53.17095540632753625, 2.595721307129207567 ) ) ;
#6719 = DIRECTION ( 'NONE',  ( -1.000000000000000000, -0.000000000000000000, -0.000000000000000000 ) ) ;
#6720 = CARTESIAN_POINT ( 'NONE',  ( 201.0270608673618256, -0.06628147382068544369, -4.392917125964748593 ) ) ;
#6721 = DIRECTION ( 'NONE',  ( 0.4084849465052255435, -0.7075166814741008503, -0.5766803221148599778 ) ) ;
#6722 = LINE ( 'NONE', #8544, #10310 ) ;
#6724 = ORIENTED_EDGE ( 'NONE', *, *, #12734, .F. ) ;
#6723 = ORIENTED_EDGE ( 'NONE', *, *, #16286, .F. ) ;
#6725 = B_SPLINE_CURVE_WITH_KNOTS ( 'NONE', 3,
 ( #19881, #13649, #15253, #2402 ),
 .UNSPECIFIED., .F., .F.,
 ( 4, 4 ),
 ( 7.737990982947961127E-05, 0.0009313656478097689061 ),
 .UNSPECIFIED. ) ;
#6726 = ORIENTED_EDGE ( 'NONE', *, *, #498, .T. ) ;
#6727 = VERTEX_POINT ( 'NONE', #14542 ) ;
#6728 = CARTESIAN_POINT ( 'NONE',  ( 204.2095024616932051, 2.543922127990230209, -25.46066938576250038 ) ) ;
#6729 = CYLINDRICAL_SURFACE ( 'NONE', #9828, 14.99999999999999645 ) ;
#6730 = ORIENTED_EDGE ( 'NONE', *, *, #4070, .F. ) ;
#6731 = ORIENTED_EDGE ( 'NONE', *, *, #7773, .T. ) ;
#6732 = EDGE_CURVE ( 'NONE', #12589, #14216, #14618, .T. ) ;
#6733 = CARTESIAN_POINT ( 'NONE',  ( 227.1431551712864803, 41.29191727552926494, -10.76535568099441420 ) ) ;
#6734 = CARTESIAN_POINT ( 'NONE',  ( 69.50490953756755630, 173.5703347563769796, 11.00000000000001243 ) ) ;
#6735 = CARTESIAN_POINT ( 'NONE',  ( 61.99529059433388767, 216.5773763115390693, -28.99999999999998934 ) ) ;
#6736 = CARTESIAN_POINT ( 'NONE',  ( 218.2868491065612488, 38.76284410478177733, -14.55761806292083982 ) ) ;
#6737 = ORIENTED_EDGE ( 'NONE', *, *, #18496, .F. ) ;
#6738 = ORIENTED_EDGE ( 'NONE', *, *, #17861, .F. ) ;
#6739 = DIRECTION ( 'NONE',  ( 0.5000000000000044409, -0.8660254037844360431, -4.006172263299080068E-16 ) ) ;
#6740 = CIRCLE ( 'NONE', #17606, 3.902363844300875240 ) ;
#6741 = ORIENTED_EDGE ( 'NONE', *, *, #16418, .F. ) ;
#6742 = AXIS2_PLACEMENT_3D ( 'NONE', #5240, #2396, #5341 ) ;
#6743 = CARTESIAN_POINT ( 'NONE',  ( 212.9202825050182923, 6.800273240212296955, -24.96223045542567931 ) ) ;
#6744 = ADVANCED_FACE ( 'NONE', ( #19666 ), #3086, .T. ) ;
#6745 = CARTESIAN_POINT ( 'NONE',  ( 42.39721438298049350, 244.5222400402098231, -18.99999999999997513 ) ) ;
#6746 = CARTESIAN_POINT ( 'NONE',  ( -28.38754368462288369, 47.74392439351031214, -1.698457930398967308 ) ) ;
#6747 = DIRECTION ( 'NONE',  ( 0.000000000000000000, -0.5000000000000013323, -0.8660254037844378194 ) ) ;
#6748 = AXIS2_PLACEMENT_3D ( 'NONE', #11541, #13042, #19693 ) ;
#6749 = VERTEX_POINT ( 'NONE', #6842 ) ;
#6750 = FACE_OUTER_BOUND ( 'NONE', #8886, .T. ) ;
#6751 = CARTESIAN_POINT ( 'NONE',  ( 208.4761278624580711, 5.007259451653140125, -14.00000000000005507 ) ) ;
#6752 = ORIENTED_EDGE ( 'NONE', *, *, #7199, .F. ) ;
#6753 = AXIS2_PLACEMENT_3D ( 'NONE', #17550, #12682, #19137 ) ;
#6754 = CARTESIAN_POINT ( 'NONE',  ( 61.60468526918592858, 83.16973256007099735, -6.383283800364179861 ) ) ;
#6755 = EDGE_CURVE ( 'NONE', #2132, #19734, #19773, .T. ) ;
#6756 = VECTOR ( 'NONE', #12549, 1000.000000000000000 ) ;
#6757 = ORIENTED_EDGE ( 'NONE', *, *, #17949, .T. ) ;
#6758 = ADVANCED_FACE ( 'NONE', ( #15040, #9525 ), #6939, .F. ) ;
#6759 = DIRECTION ( 'NONE',  ( 0.000000000000000000, 6.938893903907177533E-18, 1.000000000000000000 ) ) ;
#6760 = CARTESIAN_POINT ( 'NONE',  ( 225.9196962679179137, 42.75805112463326907, -12.51312656967076897 ) ) ;
#6761 = ORIENTED_EDGE ( 'NONE', *, *, #962, .T. ) ;
#6762 = LINE ( 'NONE', #4974, #11075 ) ;
#6763 = VECTOR ( 'NONE', #129, 1000.000000000000000 ) ;
#6764 = CARTESIAN_POINT ( 'NONE',  ( -28.22805963754889191, 65.74999999999998579, 3.997049355788913960 ) ) ;
#6765 = EDGE_CURVE ( 'NONE', #17780, #3281, #11969, .T. ) ;
#6766 = ORIENTED_EDGE ( 'NONE', *, *, #2283, .T. ) ;
#6767 = B_SPLINE_CURVE_WITH_KNOTS ( 'NONE', 3,
 ( #1359, #20533, #1048, #19166 ),
 .UNSPECIFIED., .F., .F.,
 ( 4, 4 ),
 ( 0.0001125711301185649063, 0.0007852219221655419622 ),
 .UNSPECIFIED. ) ;
#6768 = AXIS2_PLACEMENT_3D ( 'NONE', #8721, #10513, #11919 ) ;
#6769 = CARTESIAN_POINT ( 'NONE',  ( 210.5941221282246545, 5.457263920492195552, -2.233628351993232730 ) ) ;
#6770 = DIRECTION ( 'NONE',  ( 7.930164461608273850E-15, 3.965082230804136925E-15, -1.000000000000000000 ) ) ;
#6771 = CARTESIAN_POINT ( 'NONE',  ( 222.1691453665456493, 32.03850973245414480, -13.97349461567483964 ) ) ;
#6772 = CARTESIAN_POINT ( 'NONE',  ( 9.999999999999994671, 8.000000000000000000, 0.000000000000000000 ) ) ;
#6773 = ADVANCED_FACE ( 'NONE', ( #10106 ), #17649, .T. ) ;
#6774 = VECTOR ( 'NONE', #2982, 1000.000000000000227 ) ;
#6775 = ORIENTED_EDGE ( 'NONE', *, *, #8345, .T. ) ;
#6776 = LINE ( 'NONE', #331, #6763 ) ;
#6777 = DIRECTION ( 'NONE',  ( -0.3430151393149145078, -0.1980398830195854720, -0.9182161068802695558 ) ) ;
#6778 = CARTESIAN_POINT ( 'NONE',  ( 198.2719933611348040, -1.399321216369431298, -12.59769448420646043 ) ) ;
#6779 = VERTEX_POINT ( 'NONE', #10428 ) ;
#6780 = CARTESIAN_POINT ( 'NONE',  ( 221.0007431456517395, 33.44439337337441032, -11.10922658182128764 ) ) ;
#6781 = CIRCLE ( 'NONE', #11205, 11.98469917212512215 ) ;
#6782 = EDGE_CURVE ( 'NONE', #11275, #1811, #18188, .T. ) ;
#6783 = DIRECTION ( 'NONE',  ( -0.8660254037844357100, -0.5000000000000051070, 0.000000000000000000 ) ) ;
#6784 = CIRCLE ( 'NONE', #17992, 5.000000000000005329 ) ;
#6785 = ORIENTED_EDGE ( 'NONE', *, *, #17239, .T. ) ;
#6786 = CARTESIAN_POINT ( 'NONE',  ( -13.42979308546154193, 70.72677659407449369, -4.297493274131825913 ) ) ;
#6787 = AXIS2_PLACEMENT_3D ( 'NONE', #19512, #133, #16353 ) ;
#6788 = CARTESIAN_POINT ( 'NONE',  ( 79.70372278314360415, 50.44095208298563904, -16.99510208773339315 ) ) ;
#6789 = EDGE_CURVE ( 'NONE', #10758, #5372, #695, .T. ) ;
#6791 = ORIENTED_EDGE ( 'NONE', *, *, #15669, .T. ) ;
#6790 = ORIENTED_EDGE ( 'NONE', *, *, #7718, .F. ) ;
#6792 = CIRCLE ( 'NONE', #9172, 7.960520131757803597 ) ;
#6793 = ADVANCED_BREP_SHAPE_REPRESENTATION ( '', ( #10712, #18233 ), #16874 ) ;
#6794 = ORIENTED_EDGE ( 'NONE', *, *, #19895, .F. ) ;
#6795 = ORIENTED_EDGE ( 'NONE', *, *, #12686, .T. ) ;
#6796 = EDGE_CURVE ( 'NONE', #10831, #7353, #3358, .T. ) ;
#6797 = B_SPLINE_CURVE_WITH_KNOTS ( 'NONE', 3,
 ( #6907, #13392, #2362, #5414 ),
 .UNSPECIFIED., .F., .F.,
 ( 4, 4 ),
 ( 7.495004023226334094E-05, 0.0007476008322856125647 ),
 .UNSPECIFIED. ) ;
#6798 = CARTESIAN_POINT ( 'NONE',  ( 208.5840039954387066, 11.71972914181512060, -2.522505859538486828 ) ) ;
#6799 = EDGE_CURVE ( 'NONE', #2132, #14589, #6781, .T. ) ;
#6800 = VERTEX_POINT ( 'NONE', #19870 ) ;
#6801 = CARTESIAN_POINT ( 'NONE',  ( 77.00536975482934565, 54.64809360459321397, -4.630024151736636284 ) ) ;
#6802 = CARTESIAN_POINT ( 'NONE',  ( -17.04221037121256899, 79.99997668367075221, -12.46941917154160961 ) ) ;
#6803 = CARTESIAN_POINT ( 'NONE',  ( 5.000000000000004441, -3.469446951953614189E-15, -4.057500000000000107 ) ) ;
#6804 = CARTESIAN_POINT ( 'NONE',  ( 220.9861243444424304, 33.88158418318889886, -10.61701699970696211 ) ) ;
#6805 = EDGE_LOOP ( 'NONE', ( #16956, #13022, #20421, #17398, #20769 ) ) ;
#6806 = AXIS2_PLACEMENT_3D ( 'NONE', #13311, #8523, #13204 ) ;
#6807 = CARTESIAN_POINT ( 'NONE',  ( 208.4761278624580711, 5.007259451653140125, -14.00000000000005507 ) ) ;
#6808 = VECTOR ( 'NONE', #7503, 1000.000000000000114 ) ;
#6809 = EDGE_CURVE ( 'NONE', #9937, #19903, #386, .T. ) ;
#6810 = AXIS2_PLACEMENT_3D ( 'NONE', #11921, #3958, #4058 ) ;
#6811 = FACE_OUTER_BOUND ( 'NONE', #17568, .T. ) ;
#6812 = DIRECTION ( 'NONE',  ( 0.8660254037844371533, 0.5000000000000025535, 7.216449660063516527E-16 ) ) ;
#6813 = EDGE_LOOP ( 'NONE', ( #11508, #5831, #13834, #11138, #18127, #11633 ) ) ;
#6814 = CIRCLE ( 'NONE', #9522, 1.499999999999990896 ) ;
#6815 = CARTESIAN_POINT ( 'NONE',  ( 207.4656388362385826, 11.07404071609863117, -10.98795432269212391 ) ) ;
#6816 = CYLINDRICAL_SURFACE ( 'NONE', #15604, 15.00000000000001954 ) ;
#6817 = DIRECTION ( 'NONE',  ( 0.000000000000000000, 0.000000000000000000, 1.000000000000000000 ) ) ;
#6818 = CARTESIAN_POINT ( 'NONE',  ( -5.239423594773973569, 79.79422864173673702, -10.01493943371665907 ) ) ;
#6819 = ADVANCED_FACE ( 'NONE', ( #495 ), #20194, .T. ) ;
#6820=STYLED_ITEM('',(#20967),#3293);
#6822 = EDGE_LOOP ( 'NONE', ( #3600, #12155, #4199, #19281 ) ) ;
#6821 = ORIENTED_EDGE ( 'NONE', *, *, #16319, .F. ) ;
#6823 = DIRECTION ( 'NONE',  ( -0.3412765716093361656, 0.5911083614602773428, 0.7308359642781161458 ) ) ;
#6824 = CARTESIAN_POINT ( 'NONE',  ( 208.8107687779841228, 4.427644383670616079, -14.00000000000005507 ) ) ;
#6825 = VECTOR ( 'NONE', #5824, 1000.000000000000114 ) ;
#6826 = CARTESIAN_POINT ( 'NONE',  ( -32.29388722507494691, 78.35452279512254847, -5.666775083474093755 ) ) ;
#6827 = VECTOR ( 'NONE', #13191, 1000.000000000000114 ) ;
#6828 = ADVANCED_FACE ( 'NONE', ( #5336 ), #4084, .T. ) ;
#6829 = CIRCLE ( 'NONE', #9518, 3.902363844300875240 ) ;
#6830 = CARTESIAN_POINT ( 'NONE',  ( 0.000000000000000000, -2.342598717236899386, 4.057500000000001883 ) ) ;
#6831 = EDGE_CURVE ( 'NONE', #2307, #11320, #5595, .T. ) ;
#6832 = DIRECTION ( 'NONE',  ( -9.512199820426880209E-17, 4.523559531338709945E-17, -1.000000000000000000 ) ) ;
#6833 = LINE ( 'NONE', #13416, #10277 ) ;
#6834 = EDGE_LOOP ( 'NONE', ( #16517, #19878, #13153, #17698 ) ) ;
#6835 = CARTESIAN_POINT ( 'NONE',  ( 82.28441920437502688, 62.16931913188273739, -25.19187085580666974 ) ) ;
#6836 = CARTESIAN_POINT ( 'NONE',  ( 219.1503276808599594, 36.64940697350503029, -10.80501622924627902 ) ) ;
#6837 = ORIENTED_EDGE ( 'NONE', *, *, #15027, .F. ) ;
#6838 = DIRECTION ( 'NONE',  ( 0.5000000000000049960, -0.8660254037844358210, 0.000000000000000000 ) ) ;
#6839 = CARTESIAN_POINT ( 'NONE',  ( -4.055026664453261098, 55.59176219034431199, 3.696206164233441172 ) ) ;
#6840 = CARTESIAN_POINT ( 'NONE',  ( -5.615923431034060442, 79.82407219761680039, -10.19945363082080902 ) ) ;
#6841 = VECTOR ( 'NONE', #5418, 1000.000000000000114 ) ;
#6842 = CARTESIAN_POINT ( 'NONE',  ( -15.99999999999999289, 4.999999999999997335, -17.50000000000000000 ) ) ;
#6843 = DIRECTION ( 'NONE',  ( 0.2588190451025150773, 0.9659258262890698665, 8.659560562354927928E-17 ) ) ;
#6844 = PRESENTATION_LAYER_ASSIGNMENT (  '', '', ( #9552 ) ) ;
#6846 = ORIENTED_EDGE ( 'NONE', *, *, #20883, .T. ) ;
#6845 = ORIENTED_EDGE ( 'NONE', *, *, #18489, .T. ) ;
#6847 = ORIENTED_EDGE ( 'NONE', *, *, #13447, .T. ) ;
#6848 = FACE_OUTER_BOUND ( 'NONE', #630, .T. ) ;
#6849 = CARTESIAN_POINT ( 'NONE',  ( 205.8264633344831225, 9.596613037118636669, -14.00000000000005507 ) ) ;
#6850 = ORIENTED_EDGE ( 'NONE', *, *, #5585, .F. ) ;
#6851 = CARTESIAN_POINT ( 'NONE',  ( 81.73379619358640014, 63.34273602762666400, 0.3959381786365755440 ) ) ;
#6852 = PRODUCT_DEFINITION_SHAPE ( 'NONE', 'NONE',  #20960 ) ;
#6853 = CARTESIAN_POINT ( 'NONE',  ( 192.0123155716598262, 35.38128320186126530, -9.087049258353282255 ) ) ;
#6854 = DIRECTION ( 'NONE',  ( 0.8296432542242783148, 0.4789947561577510560, 0.2868032327110804358 ) ) ;
#6855 = ORIENTED_EDGE ( 'NONE', *, *, #11460, .F. ) ;
#6856 = FACE_OUTER_BOUND ( 'NONE', #1530, .T. ) ;
#6857 = DIRECTION ( 'NONE',  ( 0.000000000000000000, 0.000000000000000000, 1.000000000000000000 ) ) ;
#6858 = VECTOR ( 'NONE', #20656, 1000.000000000000000 ) ;
#6859 = B_SPLINE_CURVE_WITH_KNOTS ( 'NONE', 3,
 ( #68, #163, #8306, #4827 ),
 .UNSPECIFIED., .F., .F.,
 ( 4, 4 ),
 ( 3.603418170169278305E-07, 0.0008543460797983053016 ),
 .UNSPECIFIED. ) ;
#6860 = CARTESIAN_POINT ( 'NONE',  ( 218.8959393621077254, 37.70786883578019655, -11.12998660979001286 ) ) ;
#6861 = EDGE_CURVE ( 'NONE', #15101, #16061, #2187, .T. ) ;
#6862 = CARTESIAN_POINT ( 'NONE',  ( 61.99529059433385925, 216.5773763115390125, -5.999999999999973355 ) ) ;
#6863 = CARTESIAN_POINT ( 'NONE',  ( -28.50825147543515214, 49.06444853241422521, -0.2686478949330403654 ) ) ;
#6864 = LINE ( 'NONE', #13349, #20074 ) ;
#6865 = DIRECTION ( 'NONE',  ( -0.8660254037844357100, -0.5000000000000051070, 0.000000000000000000 ) ) ;
#6866 = FACE_OUTER_BOUND ( 'NONE', #4067, .T. ) ;
#6867 = ORIENTED_EDGE ( 'NONE', *, *, #10318, .T. ) ;
#6868 = VERTEX_POINT ( 'NONE', #9054 ) ;
#6869 = CARTESIAN_POINT ( 'NONE',  ( 58.58021009698714465, 85.49666042193958049, -12.14404289180734686 ) ) ;
#6870 = ORIENTED_EDGE ( 'NONE', *, *, #941, .T. ) ;
#6871 = VERTEX_POINT ( 'NONE', #4192 ) ;
#6872 = CARTESIAN_POINT ( 'NONE',  ( -3.348702641817554060, 65.53858748455307648, 2.490407514064874039 ) ) ;
#6873 = DIRECTION ( 'NONE',  ( 0.5000000000000045519, -0.8660254037844362651, 0.000000000000000000 ) ) ;
#6874 = EDGE_CURVE ( 'NONE', #9882, #3756, #12856, .T. ) ;
#6875 = CARTESIAN_POINT ( 'NONE',  ( 183.9132435853528023, 37.55142300003368661, -16.92893218813456002 ) ) ;
#6876 = ORIENTED_EDGE ( 'NONE', *, *, #8175, .T. ) ;
#6877 = CARTESIAN_POINT ( 'NONE',  ( 193.8427921854145097, 7.332884452518919183, -11.24974199967268262 ) ) ;
#6878 = ORIENTED_EDGE ( 'NONE', *, *, #19334, .F. ) ;
#6879 = AXIS2_PLACEMENT_3D ( 'NONE', #8920, #15520, #13914 ) ;
#6880 = APPLICATION_CONTEXT ( 'automotive_design' ) ;
#6881 = DIRECTION ( 'NONE',  ( 0.7951984747223579397, 0.4591080534401397184, -0.3960797660391670583 ) ) ;
#6882 = AXIS2_PLACEMENT_3D ( 'NONE', #14877, #5506, #5607 ) ;
#6883 = LINE ( 'NONE', #5284, #19807 ) ;
#6884 = ADVANCED_FACE ( 'NONE', ( #2716 ), #1510, .T. ) ;
#6885 = ORIENTED_EDGE ( 'NONE', *, *, #15399, .T. ) ;
#6886 = EDGE_CURVE ( 'NONE', #20843, #18617, #3199, .T. ) ;
#6887 = CARTESIAN_POINT ( 'NONE',  ( 227.5214461420562770, 40.63669809411138090, -18.16400186620061064 ) ) ;
#6888 = LINE ( 'NONE', #19816, #12285 ) ;
#6889 = EDGE_LOOP ( 'NONE', ( #18345, #11274, #20774, #266 ) ) ;
#6890 = DIRECTION ( 'NONE',  ( -0.5000000000000046629, 0.8660254037844359321, 0.000000000000000000 ) ) ;
#6891 = CARTESIAN_POINT ( 'NONE',  ( 4.000000000000000000, 3.518949890710767026, -4.987329993433320396E-15 ) ) ;
#6892 = CARTESIAN_POINT ( 'NONE',  ( 197.7473131227538659, -1.187024626400782656, -12.53629070788332989 ) ) ;
#6893 = VERTEX_POINT ( 'NONE', #18821 ) ;
#6894 = LINE ( 'NONE', #2035, #18995 ) ;
#6895 = CARTESIAN_POINT ( 'NONE',  ( 203.3234976231972553, 23.93187681866832861, -14.00000000000004441 ) ) ;
#6896 = CARTESIAN_POINT ( 'NONE',  ( 226.1710338656017996, 42.97568076809498905, -15.57898118447794822 ) ) ;
#6897 = VECTOR ( 'NONE', #5434, 1000.000000000000000 ) ;
#6898 = CARTESIAN_POINT ( 'NONE',  ( 77.93373660234723843, 52.03134620786124032, -13.52073087868893353 ) ) ;
#6899 = ORIENTED_EDGE ( 'NONE', *, *, #20447, .F. ) ;
#6900 = ORIENTED_EDGE ( 'NONE', *, *, #13935, .T. ) ;
#6901 = ADVANCED_FACE ( 'NONE', ( #14462 ), #20293, .F. ) ;
#6902 = CARTESIAN_POINT ( 'NONE',  ( 226.3860647049296517, 42.27676735321927026, -16.37421369872743071 ) ) ;
#6903 = ORIENTED_EDGE ( 'NONE', *, *, #9402, .F. ) ;
#6904 = CARTESIAN_POINT ( 'NONE',  ( 8.000000000000000000, 0.000000000000000000, 0.000000000000000000 ) ) ;
#6905 = CARTESIAN_POINT ( 'NONE',  ( -15.99999999999999289, 79.99999999999998579, -12.50000000000000000 ) ) ;
#6906 = CARTESIAN_POINT ( 'NONE',  ( 198.4513784989219971, 5.692645179619979068, -5.166194743381255172 ) ) ;
#6907 = CARTESIAN_POINT ( 'NONE',  ( 196.3264911765913041, 4.642850816258196289, -8.609703802792473937 ) ) ;
#6908 = ORIENTED_EDGE ( 'NONE', *, *, #3037, .T. ) ;
#6909 = EDGE_CURVE ( 'NONE', #15193, #2749, #2613, .T. ) ;
#6910 = CARTESIAN_POINT ( 'NONE',  ( 99.99529059433426426, 150.7594456239217777, 21.00000000000000711 ) ) ;
#6911 = SHAPE_REPRESENTATION ( 'Middle Handle-Connected Base', ( #18233 ), #10424 ) ;
#6912 = CARTESIAN_POINT ( 'NONE',  ( 54.95391741498237081, 77.69916480981964924, -15.28953269010268734 ) ) ;
#6913 = LINE ( 'NONE', #365, #3635 ) ;
#6914 = ORIENTED_EDGE ( 'NONE', *, *, #1276, .F. ) ;
#6915 = CARTESIAN_POINT ( 'NONE',  ( 218.9705756877035583, 36.93072175235232635, -11.00782313096290288 ) ) ;
#6916 = CARTESIAN_POINT ( 'NONE',  ( 10.49211908931699178, 0.000000000000000000, 0.000000000000000000 ) ) ;
#6917 = ADVANCED_FACE ( 'NONE', ( #2507 ), #11149, .T. ) ;
#6918 = DIRECTION ( 'NONE',  ( 0.5000000000000041078, -0.8660254037844363761, 0.000000000000000000 ) ) ;
#6919 = CARTESIAN_POINT ( 'NONE',  ( -13.92188866561930993, 79.99981534483862333, -12.41883285859719344 ) ) ;
#6920 = EDGE_LOOP ( 'NONE', ( #8863, #2231, #7508, #5243 ) ) ;
#6921 = CARTESIAN_POINT ( 'NONE',  ( 226.0205903126869487, 43.23625664541471281, -13.49489896056980420 ) ) ;
#6922 = DIRECTION ( 'NONE',  ( 0.000000000000000000, 0.000000000000000000, 1.000000000000000000 ) ) ;
#6923 = CARTESIAN_POINT ( 'NONE',  ( 227.6511661303252367, 39.43255059260894768, -17.89498551959673023 ) ) ;
#6924 = EDGE_CURVE ( 'NONE', #5803, #17269, #5760, .T. ) ;
#6925 = CARTESIAN_POINT ( 'NONE',  ( 79.81850713789391705, 50.75766720200975612, -17.68144038527332285 ) ) ;
#6926 = AXIS2_PLACEMENT_3D ( 'NONE', #356, #15105, #3727 ) ;
#6927 = CARTESIAN_POINT ( 'NONE',  ( -29.99999999999993605, 5.000000000000018652, 8.518881768062307458 ) ) ;
#6928 = DIRECTION ( 'NONE',  ( 0.000000000000000000, -0.5000000000000013323, -0.8660254037844378194 ) ) ;
#6929 = ORIENTED_EDGE ( 'NONE', *, *, #13487, .F. ) ;
#6930 = EDGE_CURVE ( 'NONE', #7189, #17545, #1718, .T. ) ;
#6931 = CARTESIAN_POINT ( 'NONE',  ( 82.94363963020224162, 62.33598545253519774, -25.40129762469373631 ) ) ;
#6932 = CARTESIAN_POINT ( 'NONE',  ( -3.659121735415404864, 47.49494768642473730, -2.010530405749917371 ) ) ;
#6933 = VERTEX_POINT ( 'NONE', #15449 ) ;
#6934 = DIRECTION ( 'NONE',  ( 0.5000000000000054401, -0.8660254037844354880, 0.000000000000000000 ) ) ;
#6935 = CARTESIAN_POINT ( 'NONE',  ( -3.123205458604330076, 58.78078776664096239, 1.164416042648590777 ) ) ;
#6936 = CARTESIAN_POINT ( 'NONE',  ( 1.484819526751601559, 76.25000000000000000, -2.578432583507792142 ) ) ;
#6937 = VECTOR ( 'NONE', #9273, 1000.000000000000114 ) ;
#6938 = EDGE_CURVE ( 'NONE', #15862, #3973, #9155, .T. ) ;
#6939 = PLANE ( 'NONE',  #5773 ) ;
#6940 = DIRECTION ( 'NONE',  ( -0.5000000000000051070, 0.8660254037844359321, -0.000000000000000000 ) ) ;
#6941 = LINE ( 'NONE', #8645, #2603 ) ;
#6942 = EDGE_CURVE ( 'NONE', #17033, #6453, #1342, .T. ) ;
#6944 = VERTEX_POINT ( 'NONE', #7572 ) ;
#6943 = ORIENTED_EDGE ( 'NONE', *, *, #13888, .T. ) ;
#6945 = ORIENTED_EDGE ( 'NONE', *, *, #14764, .F. ) ;
#6946 = TOROIDAL_SURFACE ( 'NONE', #3579, 17.50000000000000000, 5.000000000000000000 ) ;
#6947 = VERTEX_POINT ( 'NONE', #15556 ) ;
#6948 = CARTESIAN_POINT ( 'NONE',  ( 229.5841978618468033, 37.06390731203416777, -15.46846178913027714 ) ) ;
#6949 = CARTESIAN_POINT ( 'NONE',  ( -11.68625644715183931, 64.25000000000000000, -2.528164662410438357 ) ) ;
#6950 = ORIENTED_EDGE ( 'NONE', *, *, #8206, .F. ) ;
#6951 = ORIENTED_EDGE ( 'NONE', *, *, #4235, .T. ) ;
#6952 = CARTESIAN_POINT ( 'NONE',  ( 80.83948132674352394, 60.42342883285770938, -0.3256906176670446573 ) ) ;
#6953 = DIRECTION ( 'NONE',  ( 1.000000000000000000, -0.000000000000000000, -0.000000000000000000 ) ) ;
#6954 = PLANE ( 'NONE',  #1247 ) ;
#6955 = ORIENTED_EDGE ( 'NONE', *, *, #15291, .T. ) ;
#6956 = EDGE_CURVE ( 'NONE', #8118, #11210, #20497, .T. ) ;
#6957 = CARTESIAN_POINT ( 'NONE',  ( 62.36389338619030553, 105.9389375482328006, -12.50000000000000000 ) ) ;
#6958 = DIRECTION ( 'NONE',  ( -0.8660254037844354880, -0.5000000000000055511, 0.000000000000000000 ) ) ;
#6959 = VERTEX_POINT ( 'NONE', #9652 ) ;
#6960 = AXIS2_PLACEMENT_3D ( 'NONE', #1599, #2435, #2544 ) ;
#6961 = AXIS2_PLACEMENT_3D ( 'NONE', #17916, #20768, #12627 ) ;
#6962 = CYLINDRICAL_SURFACE ( 'NONE', #11146, 5.000000000000001776 ) ;
#6963 = EDGE_CURVE ( 'NONE', #13750, #4880, #13955, .T. ) ;
#6964 = DIRECTION ( 'NONE',  ( 0.6946590618905411629, 0.4010615963775225890, -0.5971585917027958379 ) ) ;
#6965 = CARTESIAN_POINT ( 'NONE',  ( -32.68402340442658982, 50.97242918334629280, -7.141224787959053799 ) ) ;
#6966 = DIRECTION ( 'NONE',  ( 0.7739085681710337061, 0.4468163201617106339, -0.4487991802004634989 ) ) ;
#6967 = VERTEX_POINT ( 'NONE', #4681 ) ;
#6968 = CARTESIAN_POINT ( 'NONE',  ( 188.7053703664960551, 14.98146631279701602, -16.89203719259486647 ) ) ;
#6969 = DIRECTION ( 'NONE',  ( 0.000000000000000000, 0.000000000000000000, -1.000000000000000000 ) ) ;
#6971 = ORIENTED_EDGE ( 'NONE', *, *, #14731, .F. ) ;
#6970 = ORIENTED_EDGE ( 'NONE', *, *, #9586, .F. ) ;
#6972 = AXIS2_PLACEMENT_3D ( 'NONE', #19940, #5409, #16772 ) ;
#6973 = CARTESIAN_POINT ( 'NONE',  ( 54.27365823804359479, 77.98814336746363551, -11.88731395325653040 ) ) ;
#6974 = ORIENTED_EDGE ( 'NONE', *, *, #3442, .T. ) ;
#6975 = VERTEX_POINT ( 'NONE', #17625 ) ;
#6976 = CIRCLE ( 'NONE', #12745, 11.94520687646042667 ) ;
#6977 = CARTESIAN_POINT ( 'NONE',  ( 218.5623757963967080, 10.31533654458964477, -18.15054426878737104 ) ) ;
#6978 = CIRCLE ( 'NONE', #13428, 11.94520687646042667 ) ;
#6979 = CYLINDRICAL_SURFACE ( 'NONE', #5941, 3.902363844300889451 ) ;
#6980 = B_SPLINE_CURVE_WITH_KNOTS ( 'NONE', 3,
 ( #5338, #13427, #2084, #16597 ),
 .UNSPECIFIED., .F., .F.,
 ( 4, 4 ),
 ( 2.451646831110292017E-05, 0.0008785022062956360364 ),
 .UNSPECIFIED. ) ;
#6981 = ORIENTED_EDGE ( 'NONE', *, *, #10160, .F. ) ;
#6982 = CARTESIAN_POINT ( 'NONE',  ( 41.50490953756720813, 222.0677573683055925, -14.00000000000002842 ) ) ;
#6983 = CARTESIAN_POINT ( 'NONE',  ( 219.4777721068107041, 36.49412689447730429, -10.43783272703042719 ) ) ;
#6984 = VERTEX_POINT ( 'NONE', #9551 ) ;
#6985 = PLANE ( 'NONE',  #9436 ) ;
#6986 = CARTESIAN_POINT ( 'NONE',  ( 205.0662616026534693, 10.91332106064940888, -14.00000000000005507 ) ) ;
#6987 = VECTOR ( 'NONE', #8149, 1000.000000000000227 ) ;
#6988 = ORIENTED_EDGE ( 'NONE', *, *, #15224, .T. ) ;
#6989 = DIRECTION ( 'NONE',  ( 0.5000000000000054401, -0.8660254037844354880, 0.000000000000000000 ) ) ;
#6990 = CARTESIAN_POINT ( 'NONE',  ( -29.99999999999999645, 5.000000000000000000, 15.00000000000000000 ) ) ;
#6991 = CARTESIAN_POINT ( 'NONE',  ( 213.6457381091975662, 14.64212269496015750, -5.449056122693788140 ) ) ;
#6992 = ORIENTED_EDGE ( 'NONE', *, *, #6672, .F. ) ;
#6993 = LINE ( 'NONE', #8591, #8467 ) ;
#6994 = PLANE ( 'NONE',  #5867 ) ;
#6995 = CARTESIAN_POINT ( 'NONE',  ( 5.000000000000000000, 7.027796151710712813, -4.057500000000007212 ) ) ;
#6996 = ORIENTED_EDGE ( 'NONE', *, *, #18939, .T. ) ;
#6997 = CARTESIAN_POINT ( 'NONE',  ( 82.92574498128803384, 61.78441515947673679, 0.3082669428048712135 ) ) ;
#6998 = CARTESIAN_POINT ( 'NONE',  ( -4.239935945710826104, 64.25000000000000000, 4.526879896143025661 ) ) ;
#6999 = PLANE ( 'NONE',  #2225 ) ;
#7001 = VERTEX_POINT ( 'NONE', #6360 ) ;
#7000 = VERTEX_POINT ( 'NONE', #16048 ) ;
#7002 = VECTOR ( 'NONE', #6739, 1000.000000000000114 ) ;
#7003 = EDGE_CURVE ( 'NONE', #10831, #13023, #8054, .T. ) ;
#7004 = CIRCLE ( 'NONE', #4646, 11.98469917212512215 ) ;
#7005 = DIRECTION ( 'NONE',  ( 0.000000000000000000, -1.000000000000000000, 0.000000000000000000 ) ) ;
#7006 = VERTEX_POINT ( 'NONE', #12964 ) ;
#7007 = CONICAL_SURFACE ( 'NONE', #13129, 10.85470691220533190, 0.8171114040043576665 ) ;
#7008 = LINE ( 'NONE', #14890, #9679 ) ;
#7009 = ORIENTED_EDGE ( 'NONE', *, *, #14237, .F. ) ;
#7010 = CARTESIAN_POINT ( 'NONE',  ( 184.9952905943350459, 3.535126980567737665, -6.000000000000071942 ) ) ;
#7011 = CARTESIAN_POINT ( 'NONE',  ( -23.54107059693361492, 80.00000000014368595, -10.01181548797457488 ) ) ;
#7012 = CARTESIAN_POINT ( 'NONE',  ( 0.000000000000000000, -10.00000000000000000, -30.00000000000000000 ) ) ;
#7013 = CARTESIAN_POINT ( 'NONE',  ( 218.1074424443701503, 10.31028766640382344, -8.485309299592367793 ) ) ;
#7014 = ORIENTED_EDGE ( 'NONE', *, *, #12775, .T. ) ;
#7015 = DIRECTION ( 'NONE',  ( 0.5000000000000053291, -0.8660254037844354880, 0.000000000000000000 ) ) ;
#7016 = ADVANCED_FACE ( 'NONE', ( #19411 ), #10538, .T. ) ;
#7017 = CARTESIAN_POINT ( 'NONE',  ( 203.2336538649942668, 12.75470097114692969, -25.81526893633797570 ) ) ;
#7018 = AXIS2_PLACEMENT_3D ( 'NONE', #9893, #6832, #19547 ) ;
#7019 = CARTESIAN_POINT ( 'NONE',  ( 222.1491677973493495, 32.07311189731386492, -14.55761806292095706 ) ) ;
#7020 = PRODUCT_DEFINITION_SHAPE ( 'NONE', 'NONE',  #20959 ) ;
#7021 = ORIENTED_EDGE ( 'NONE', *, *, #1210, .T. ) ;
#7023 = DIRECTION ( 'NONE',  ( 0.04526787302125637180, -0.07840625602339144906, 0.9958932064677044060 ) ) ;
#7022 = CONICAL_SURFACE ( 'NONE', #16524, 10.85470691220533190, 0.8171114040043576665 ) ;
#7024 = DIRECTION ( 'NONE',  ( 0.000000000000000000, 0.000000000000000000, -1.000000000000000000 ) ) ;
#7025 = CARTESIAN_POINT ( 'NONE',  ( -5.550616763087108829, 79.57013539180735506, -8.777265990090908687 ) ) ;
#7026 = EDGE_CURVE ( 'NONE', #9010, #17344, #18301, .T. ) ;
#7028 = EDGE_LOOP ( 'NONE', ( #20420, #9616, #11441, #1826 ) ) ;
#7027 = ORIENTED_EDGE ( 'NONE', *, *, #18745, .F. ) ;
#7029 = VERTEX_POINT ( 'NONE', #444 ) ;
#7030 = EDGE_CURVE ( 'NONE', #7908, #18515, #12212, .T. ) ;
#7031 = CARTESIAN_POINT ( 'NONE',  ( 202.6756539743620920, 0.8855342002901112064, -23.47937149798923073 ) ) ;
#7032 = CARTESIAN_POINT ( 'NONE',  ( 5.000000000000000000, 3.513898075855357295, -2.028750000000006271 ) ) ;
#7033 = CARTESIAN_POINT ( 'NONE',  ( 209.7467543128910847, 12.39104335059658091, -13.30618937499484922 ) ) ;
#7034 = CARTESIAN_POINT ( 'NONE',  ( 82.74544973607177667, 63.95453548303478897, -25.58011531139869632 ) ) ;
#7035 =( GEOMETRIC_REPRESENTATION_CONTEXT ( 3 ) GLOBAL_UNCERTAINTY_ASSIGNED_CONTEXT ( ( #9765 ) ) GLOBAL_UNIT_ASSIGNED_CONTEXT ( ( #4906, #9671, #1943 ) ) REPRESENTATION_CONTEXT ( 'NONE', 'WORKASPACE' ) );
#7036 =( NAMED_UNIT ( * ) PLANE_ANGLE_UNIT ( ) SI_UNIT ( $, .RADIAN. ) );
#7037 = FACE_OUTER_BOUND ( 'NONE', #9296, .T. ) ;
#7038 = ORIENTED_EDGE ( 'NONE', *, *, #14627, .F. ) ;
#7039 = AXIS2_PLACEMENT_3D ( 'NONE', #7568, #15554, #14279 ) ;
#7040 = EDGE_CURVE ( 'NONE', #4535, #12762, #3608, .T. ) ;
#7041 = CARTESIAN_POINT ( 'NONE',  ( 79.51181077588671542, 55.06802793803193197, -20.92898252978093865 ) ) ;
#7042 = DIRECTION ( 'NONE',  ( -0.6299240516454520655, -0.3636868207865263658, 0.6862416378687372642 ) ) ;
#7043 = ORIENTED_EDGE ( 'NONE', *, *, #8345, .F. ) ;
#7044 = CARTESIAN_POINT ( 'NONE',  ( 26.99999999999999645, 65.74999999999995737, -2.528164662410434804 ) ) ;
#7045 = CARTESIAN_POINT ( 'NONE',  ( -3.575197966166810737, 53.09951303229428987, -3.365123708265559621 ) ) ;
#7046 = DIRECTION ( 'NONE',  ( -0.8660254037844360431, -0.5000000000000044409, 5.976026924694052093E-17 ) ) ;
#7047 = EDGE_CURVE ( 'NONE', #1811, #20230, #6776, .T. ) ;
#7048 = CARTESIAN_POINT ( 'NONE',  ( 218.2832399571946667, 38.76909533485677173, -13.49489896056980420 ) ) ;
#7049 = DIRECTION ( 'NONE',  ( -0.3886714912512297393, -0.2243995901002339699, -0.8936326403234117199 ) ) ;
#7050 = CARTESIAN_POINT ( 'NONE',  ( 208.8107687779841228, 4.427644383670616079, -14.00000000000005507 ) ) ;
#7051 = AXIS2_PLACEMENT_3D ( 'NONE', #8259, #7854, #19304 ) ;
#7053 = ORIENTED_EDGE ( 'NONE', *, *, #19181, .T. ) ;
#7052 = EDGE_LOOP ( 'NONE', ( #8810, #6524, #17718, #18197 ) ) ;
#7054 = EDGE_LOOP ( 'NONE', ( #15001, #917, #16610, #8454, #7498 ) ) ;
#7055 = CARTESIAN_POINT ( 'NONE',  ( 221.7353300886072134, 32.16953139321172728, -13.96731517339631168 ) ) ;
#7056 = CARTESIAN_POINT ( 'NONE',  ( 212.4556053886519749, 4.037449897911128183, -14.00000000000005507 ) ) ;
#7057 = ADVANCED_FACE ( 'NONE', ( #19506 ), #3302, .F. ) ;
#7058 = CARTESIAN_POINT ( 'NONE',  ( 32.39721438298032297, 261.8427481158985870, -5.999999999999973355 ) ) ;
#7059 = ORIENTED_EDGE ( 'NONE', *, *, #18100, .F. ) ;
#7060 = ORIENTED_EDGE ( 'NONE', *, *, #10562, .T. ) ;
#7061 = ORIENTED_EDGE ( 'NONE', *, *, #2834, .F. ) ;
#7062 = CARTESIAN_POINT ( 'NONE',  ( -35.00000000000000000, 64.25000000000000000, 1.479896280015796650 ) ) ;
#7063 = DIRECTION ( 'NONE',  ( -0.5000000000000008882, 0.8660254037844381525, 0.000000000000000000 ) ) ;
#7064 = CARTESIAN_POINT ( 'NONE',  ( 104.7973891242897650, 32.44196698708787352, -12.50000000000000000 ) ) ;
#7065 = ORIENTED_EDGE ( 'NONE', *, *, #1755, .F. ) ;
#7066 = DIRECTION ( 'NONE',  ( -1.000000000000000000, 0.000000000000000000, 1.129794457510891260E-16 ) ) ;
#7067 = CARTESIAN_POINT ( 'NONE',  ( 177.4952905943348753, 16.52550803733426577, -14.00000000000000533 ) ) ;
#7068 = ADVANCED_FACE ( 'NONE', ( #16347 ), #14602, .T. ) ;
#7069 = ORIENTED_EDGE ( 'NONE', *, *, #11206, .T. ) ;
#7070 = EDGE_CURVE ( 'NONE', #1958, #2325, #6993, .T. ) ;
#7071 = VECTOR ( 'NONE', #1583, 1000.000000000000000 ) ;
#7072 = CARTESIAN_POINT ( 'NONE',  ( -15.99999999999999289, 64.25000000000000000, 0.000000000000000000 ) ) ;
#7073 = DIRECTION ( 'NONE',  ( 1.000000000000000000, 0.000000000000000000, 0.000000000000000000 ) ) ;
#7074 = CARTESIAN_POINT ( 'NONE',  ( -26.27766216112225095, 45.15629102170652232, -7.122914202326710686 ) ) ;
#7075 = DIRECTION ( 'NONE',  ( 0.8660254037844355990, 0.5000000000000054401, 0.000000000000000000 ) ) ;
#7076 = EDGE_CURVE ( 'NONE', #10243, #8938, #5289, .T. ) ;
#7077 = ORIENTED_EDGE ( 'NONE', *, *, #1741, .T. ) ;
#7078 = LINE ( 'NONE', #13561, #1118 ) ;
#7079 = CARTESIAN_POINT ( 'NONE',  ( 209.3909370991932235, 3.422763374394450775, -14.00000000000005507 ) ) ;
#7081 = ORIENTED_EDGE ( 'NONE', *, *, #2558, .T. ) ;
#7080 = ORIENTED_EDGE ( 'NONE', *, *, #8372, .F. ) ;
#7082 = CARTESIAN_POINT ( 'NONE',  ( 54.32373986521573528, 77.96687596514310314, -13.46425722430111982 ) ) ;
#7083 = ORIENTED_EDGE ( 'NONE', *, *, #7992, .T. ) ;
#7084 = CIRCLE ( 'NONE', #5051, 11.98469917212512215 ) ;
#7085 = ORIENTED_EDGE ( 'NONE', *, *, #11686, .T. ) ;
#7086 = ORIENTED_EDGE ( 'NONE', *, *, #2153, .T. ) ;
#7087 = B_SPLINE_CURVE_WITH_KNOTS ( 'NONE', 3,
 ( #11423, #17789, #19376, #3361 ),
 .UNSPECIFIED., .F., .F.,
 ( 4, 4 ),
 ( 0.0001237509890165146265, 0.0007964017810610974930 ),
 .UNSPECIFIED. ) ;
#7088 = CARTESIAN_POINT ( 'NONE',  ( 5.000000000000004441, -2.342598717236910044, -4.057499999999996554 ) ) ;
#7089 = FACE_OUTER_BOUND ( 'NONE', #7052, .T. ) ;
#7090 = EDGE_CURVE ( 'NONE', #19498, #18324, #6565, .T. ) ;
#7091 = ORIENTED_EDGE ( 'NONE', *, *, #5112, .F. ) ;
#7092 = DIRECTION ( 'NONE',  ( 0.8660254037844380415, 0.5000000000000014433, 0.000000000000000000 ) ) ;
#7093 = CIRCLE ( 'NONE', #6397, 9.999999999999994671 ) ;
#7094 = FACE_OUTER_BOUND ( 'NONE', #15389, .T. ) ;
#7095 = DIRECTION ( 'NONE',  ( -0.5000000000000041078, 0.8660254037844363761, 0.000000000000000000 ) ) ;
#7096 = CARTESIAN_POINT ( 'NONE',  ( 218.8469426460937939, 37.58675557135033074, -11.20506451332624920 ) ) ;
#7097 = CARTESIAN_POINT ( 'NONE',  ( 20.67255043510014900, 151.1504617752989361, -12.49999999999999822 ) ) ;
#7098 = LINE ( 'NONE', #19815, #10331 ) ;
#7099 = CARTESIAN_POINT ( 'NONE',  ( 218.6326489791658503, 10.87112965241456841, -18.25196083293883120 ) ) ;
#7100 = EDGE_LOOP ( 'NONE', ( #16429, #10555, #4427, #12723 ) ) ;
#7101 = DIRECTION ( 'NONE',  ( -1.000000000000000000, -0.000000000000000000, -0.000000000000000000 ) ) ;
#7102 = VECTOR ( 'NONE', #3657, 1000.000000000000227 ) ;
#7103 = DIRECTION ( 'NONE',  ( 0.4999999999999995004, -0.8660254037844390407, 0.000000000000000000 ) ) ;
#7104 = DIRECTION ( 'NONE',  ( -0.8660254037844378194, -0.5000000000000013323, -0.000000000000000000 ) ) ;
#7105 = ORIENTED_EDGE ( 'NONE', *, *, #1084, .T. ) ;
#7106 = CARTESIAN_POINT ( 'NONE',  ( 81.10922206268567436, 58.43639235104441809, -1.256738101660075380 ) ) ;
#7107 = VERTEX_POINT ( 'NONE', #18242 ) ;
#7108 = DIRECTION ( 'NONE',  ( -0.5000000000000053291, 0.8660254037844354880, 0.000000000000000000 ) ) ;
#7109 = CARTESIAN_POINT ( 'NONE',  ( 79.45107170937350816, 54.94789128765694386, -4.214488722304810864 ) ) ;
#7111 = ORIENTED_EDGE ( 'NONE', *, *, #15060, .F. ) ;
#7110 = ORIENTED_EDGE ( 'NONE', *, *, #20279, .F. ) ;
#7112 = APPLICATION_PROTOCOL_DEFINITION ( 'draft international standard', 'automotive_design', 1998, #1206 ) ;
#7113 = AXIS2_PLACEMENT_3D ( 'NONE', #13507, #19954, #4275 ) ;
#7114 = AXIS2_PLACEMENT_3D ( 'NONE', #18926, #1333, #4401 ) ;
#7115 = DIRECTION ( 'NONE',  ( -1.000000000000000000, -0.000000000000000000, -0.000000000000000000 ) ) ;
#7116 = ORIENTED_EDGE ( 'NONE', *, *, #9528, .T. ) ;
#7117 = DIRECTION ( 'NONE',  ( -0.8660254037844361541, -0.5000000000000045519, 5.976026924694053325E-17 ) ) ;
#7118 = CARTESIAN_POINT ( 'NONE',  ( 199.2144802262915846, 21.04890371929339921, -14.00000000000005507 ) ) ;
#7119 = PLANE ( 'NONE',  #15142 ) ;
#7120 = CARTESIAN_POINT ( 'NONE',  ( 200.8534188064670900, 11.38047161937165974, -2.669358488461094137 ) ) ;
#7121 = EDGE_LOOP ( 'NONE', ( #8401, #19843, #969, #14598 ) ) ;
#7122 = CARTESIAN_POINT ( 'NONE',  ( 207.8344881237125890, 4.636808575765666518, -26.45271578590683248 ) ) ;
#7123 = DIRECTION ( 'NONE',  ( -0.8660254037844361541, -0.5000000000000042188, 0.000000000000000000 ) ) ;
#7124 = EDGE_CURVE ( 'NONE', #11414, #8535, #19633, .T. ) ;
#7125 = CARTESIAN_POINT ( 'NONE',  ( 198.8278877809574965, -0.5631545566074300790, -19.61257667712936126 ) ) ;
#7126 = ORIENTED_EDGE ( 'NONE', *, *, #18283, .F. ) ;
#7127 = AXIS2_PLACEMENT_3D ( 'NONE', #1779, #19269, #6626 ) ;
#7128 = DIRECTION ( 'NONE',  ( 0.5000000000000007772, -0.8660254037844381525, 0.000000000000000000 ) ) ;
#7129 = DIRECTION ( 'NONE',  ( 0.5000000000000045519, -0.8660254037844360431, -4.006172263299080561E-16 ) ) ;
#7130 = CONICAL_SURFACE ( 'NONE', #718, 4.509097725792825528, 0.5235987755983015912 ) ;
#7131 = DIRECTION ( 'NONE',  ( -0.5000000000000008882, 0.8660254037844381525, 0.000000000000000000 ) ) ;
#7132 = CARTESIAN_POINT ( 'NONE',  ( 229.8305667389344933, 36.63718389951434773, -12.92165662794199577 ) ) ;
#7133 = AXIS2_PLACEMENT_3D ( 'NONE', #10973, #7984, #12680 ) ;
#7134 = ORIENTED_EDGE ( 'NONE', *, *, #19402, .F. ) ;
#7135 = ORIENTED_EDGE ( 'NONE', *, *, #8504, .F. ) ;
#7136 = DIRECTION ( 'NONE',  ( -0.8660254037844355990, -0.5000000000000053291, 0.000000000000000000 ) ) ;
#7137 = CARTESIAN_POINT ( 'NONE',  ( 5.000000000000004441, 7.027796151710827388, -4.057500000000009877 ) ) ;
#7138 = DIRECTION ( 'NONE',  ( 0.000000000000000000, 0.000000000000000000, -1.000000000000000000 ) ) ;
#7139 = AXIS2_PLACEMENT_3D ( 'NONE', #14600, #17973, #17874 ) ;
#7140 = CARTESIAN_POINT ( 'NONE',  ( 82.32810266468291616, 65.12101312253520291, -25.63465024353788735 ) ) ;
#7141 = CARTESIAN_POINT ( 'NONE',  ( -28.06876874214889384, 9.090108580520308124, 3.321481296491451740 ) ) ;
#7142 = AXIS2_PLACEMENT_3D ( 'NONE', #7994, #12996, #9473 ) ;
#7143 = CARTESIAN_POINT ( 'NONE',  ( 205.5965122587965084, 9.994899983462953941, -14.00000000000005507 ) ) ;
#7144 = ORIENTED_EDGE ( 'NONE', *, *, #6551, .T. ) ;
#7145 = AXIS2_PLACEMENT_3D ( 'NONE', #13967, #1441, #15667 ) ;
#7146 = CARTESIAN_POINT ( 'NONE',  ( 81.82243405374090628, 65.98882302804530298, -25.63369653231234224 ) ) ;
#7147 = CARTESIAN_POINT ( 'NONE',  ( 59.14661261761333577, 85.06148897809092091, -15.22085364341173275 ) ) ;
#7148 = EDGE_CURVE ( 'NONE', #17136, #10069, #20322, .T. ) ;
#7149 = ORIENTED_EDGE ( 'NONE', *, *, #10975, .T. ) ;
#7150 = EDGE_CURVE ( 'NONE', #14393, #122, #1712, .T. ) ;
#7151 = CARTESIAN_POINT ( 'NONE',  ( 27.66662763442663575, 65.75000000000001421, -1.859747928060466293 ) ) ;
#7152 = CARTESIAN_POINT ( 'NONE',  ( 198.7478178127443016, -1.382203064952688409, -11.23040475586387821 ) ) ;
#7153 = CARTESIAN_POINT ( 'NONE',  ( 228.1724852575672458, 39.18259619236566493, -10.35599826740967799 ) ) ;
#7154 = CARTESIAN_POINT ( 'NONE',  ( 97.97831163141611910, 199.4916918115227702, 8.754184836083465981 ) ) ;
#7155 = PLANE ( 'NONE',  #9639 ) ;
#7157 = VERTEX_POINT ( 'NONE', #19717 ) ;
#7156 = ORIENTED_EDGE ( 'NONE', *, *, #39, .F. ) ;
#7158 = ORIENTED_EDGE ( 'NONE', *, *, #2033, .T. ) ;
#7159 = AXIS2_PLACEMENT_3D ( 'NONE', #13798, #2347, #13373 ) ;
#7160 = ORIENTED_EDGE ( 'NONE', *, *, #9514, .T. ) ;
#7161 = LINE ( 'NONE', #17134, #4103 ) ;
#7163 = CARTESIAN_POINT ( 'NONE',  ( 32.39721438298033007, 261.8427481158985302, -5.999999999999973355 ) ) ;
#7162 = AXIS2_PLACEMENT_3D ( 'NONE', #6065, #7556, #12560 ) ;
#7164 = AXIS2_PLACEMENT_3D ( 'NONE', #16652, #8691, #8999 ) ;
#7165 = ORIENTED_EDGE ( 'NONE', *, *, #9087, .T. ) ;
#7166 = PRESENTATION_STYLE_ASSIGNMENT (( #19784 ) ) ;
#7167 = CARTESIAN_POINT ( 'NONE',  ( 208.9378540577313004, 11.39297530874010000, -25.94618751764496878 ) ) ;
#7168 = DIRECTION ( 'NONE',  ( 1.000000000000000000, 0.000000000000000000, 0.000000000000000000 ) ) ;
#7169 =( REPRESENTATION_RELATIONSHIP ('NONE','NONE', #4634, #16277 ) REPRESENTATION_RELATIONSHIP_WITH_TRANSFORMATION ( #7640 )SHAPE_REPRESENTATION_RELATIONSHIP( ) );
#7170 = ORIENTED_EDGE ( 'NONE', *, *, #9457, .F. ) ;
#7171 = CARTESIAN_POINT ( 'NONE',  ( 220.3453756550692617, 33.06601677626848357, -11.10922658182128941 ) ) ;
#7172 = PRODUCT_DEFINITION ( 'UNKNOWN', '', #1325, #12355 ) ;
#7173 = CARTESIAN_POINT ( 'NONE',  ( 204.9818247258934321, 9.640009970873842704, -2.036337243043272238 ) ) ;
#7174 = EDGE_CURVE ( 'NONE', #18175, #14788, #11191, .T. ) ;
#7175 = DIRECTION ( 'NONE',  ( -0.8660254037844354880, -0.5000000000000055511, 0.000000000000000000 ) ) ;
#7176 = VECTOR ( 'NONE', #3842, 999.9999999999998863 ) ;
#7177 = EDGE_CURVE ( 'NONE', #844, #19176, #6669, .T. ) ;
#7178 = MECHANICAL_DESIGN_GEOMETRIC_PRESENTATION_REPRESENTATION (  '', ( #19045 ), #7194 ) ;
#7179 = DIRECTION ( 'NONE',  ( 0.5000000000000041078, -0.8660254037844361541, 0.000000000000000000 ) ) ;
#7180 = CARTESIAN_POINT ( 'NONE',  ( -17.93384870776856133, 50.46031766474980884, -16.18952312236656255 ) ) ;
#7181 = CARTESIAN_POINT ( 'NONE',  ( 219.8596994420544206, 35.21110819772841438, -14.00000000000005507 ) ) ;
#7182 = CIRCLE ( 'NONE', #9875, 4.057500000000000107 ) ;
#7183 = EDGE_CURVE ( 'NONE', #11306, #3323, #11674, .T. ) ;
#7184 = CARTESIAN_POINT ( 'NONE',  ( 201.7640869814541134, 0.3592407515502875626, -5.407152407593845744 ) ) ;
#7185 = DIRECTION ( 'NONE',  ( -0.4586056507527294102, 0.7943282877419115540, 0.3984010898462361783 ) ) ;
#7186 = ORIENTED_EDGE ( 'NONE', *, *, #824, .F. ) ;
#7187 = CARTESIAN_POINT ( 'NONE',  ( 56.96510188438568889, 76.84332181286218599, -17.86482079344752094 ) ) ;
#7188 = ORIENTED_EDGE ( 'NONE', *, *, #20111, .T. ) ;
#7189 = VERTEX_POINT ( 'NONE', #18136 ) ;
#7190 = EDGE_CURVE ( 'NONE', #20014, #1893, #13164, .T. ) ;
#7191 = VERTEX_POINT ( 'NONE', #5087 ) ;
#7192 = LINE ( 'NONE', #10360, #16953 ) ;
#7193 = FACE_OUTER_BOUND ( 'NONE', #11584, .T. ) ;
#7194 =( GEOMETRIC_REPRESENTATION_CONTEXT ( 3 ) GLOBAL_UNCERTAINTY_ASSIGNED_CONTEXT ( ( #12765 ) ) GLOBAL_UNIT_ASSIGNED_CONTEXT ( ( #19260, #1869, #5033 ) ) REPRESENTATION_CONTEXT ( 'NONE', 'WORKASPACE' ) );
#7195 = ORIENTED_EDGE ( 'NONE', *, *, #7190, .F. ) ;
#7196 = ORIENTED_EDGE ( 'NONE', *, *, #8959, .F. ) ;
#7197 = DIRECTION ( 'NONE',  ( 0.4999999999999995004, -0.8660254037844390407, 0.000000000000000000 ) ) ;
#7198 = ORIENTED_EDGE ( 'NONE', *, *, #19283, .T. ) ;
#7199 = EDGE_CURVE ( 'NONE', #20103, #4518, #11569, .T. ) ;
#7200 = CARTESIAN_POINT ( 'NONE',  ( 229.1828198488191219, 37.75911442363916137, -10.52647298641115547 ) ) ;
#7201 = CARTESIAN_POINT ( 'NONE',  ( 0.000000000000000000, -1.759474945355387954, -3.047499999999997211 ) ) ;
#7202 = PRODUCT_DEFINITION_SHAPE ( 'NONE', 'NONE',  #20953 ) ;
#7203 = LINE ( 'NONE', #4243, #2348 ) ;
#7204 = DIRECTION ( 'NONE',  ( 0.8660254037844372643, 0.5000000000000023315, 6.106226635438360972E-16 ) ) ;
#7205 = DIRECTION ( 'NONE',  ( 0.8660254037844355990, 0.5000000000000054401, 4.449885457462577074E-15 ) ) ;
#7206 = CARTESIAN_POINT ( 'NONE',  ( 199.1867014016590076, -1.128813506749884343, -18.06789442459577799 ) ) ;
#7207 = EDGE_CURVE ( 'NONE', #2978, #12472, #10849, .T. ) ;
#7208 = EDGE_CURVE ( 'NONE', #2903, #772, #4069, .T. ) ;
#7209 = VECTOR ( 'NONE', #8027, 1000.000000000000000 ) ;
#7210 = ORIENTED_EDGE ( 'NONE', *, *, #8358, .T. ) ;
#7211 = DIRECTION ( 'NONE',  ( 0.000000000000000000, 1.224646799147353207E-16, 1.000000000000000000 ) ) ;
#7212 = FACE_OUTER_BOUND ( 'NONE', #8758, .T. ) ;
#7213 = DIRECTION ( 'NONE',  ( 0.5000000000000007772, -0.8660254037844381525, 0.000000000000000000 ) ) ;
#7214 = ORIENTED_EDGE ( 'NONE', *, *, #20234, .T. ) ;
#7215 = CARTESIAN_POINT ( 'NONE',  ( 32.36389338619004263, 157.9004617752989930, -12.50000000000000000 ) ) ;
#7216 = EDGE_CURVE ( 'NONE', #12547, #14158, #5822, .T. ) ;
#7217 = ORIENTED_EDGE ( 'NONE', *, *, #14063, .F. ) ;
#7218 = CARTESIAN_POINT ( 'NONE',  ( 33.42607121268109438, 170.0607158131433607, 11.00000000000001243 ) ) ;
#7219 = LINE ( 'NONE', #20152, #10683 ) ;
#7220 = AXIS2_PLACEMENT_3D ( 'NONE', #3041, #19157, #14510 ) ;
#7221 = EDGE_CURVE ( 'NONE', #14920, #17008, #5671, .T. ) ;
#7222 = CARTESIAN_POINT ( 'NONE',  ( 229.3736054848727690, 37.42866400863998422, -11.75146085096538862 ) ) ;
#7223 = EDGE_LOOP ( 'NONE', ( #10410, #3210, #17222, #7383 ) ) ;
#7224 = CARTESIAN_POINT ( 'NONE',  ( 77.94019217027455682, 55.93687283931910770, -21.83955200455485723 ) ) ;
#7225 = CARTESIAN_POINT ( 'NONE',  ( -21.44969027868145162, 80.00000000004207834, -11.26030642047179420 ) ) ;
#7226 = CYLINDRICAL_SURFACE ( 'NONE', #18460, 3.902363844300889451 ) ;
#7227 = CARTESIAN_POINT ( 'NONE',  ( 221.7369802378075860, 32.16919332334362025, -13.95097276009443910 ) ) ;
#7228 = ORIENTED_EDGE ( 'NONE', *, *, #15109, .F. ) ;
#7229 = CARTESIAN_POINT ( 'NONE',  ( 209.3577037357181894, 3.480325248439696040, -14.00000000000005507 ) ) ;
#7230 = EDGE_CURVE ( 'NONE', #4177, #16336, #18668, .T. ) ;
#7231 = LINE ( 'NONE', #18584, #12283 ) ;
#7232 = CARTESIAN_POINT ( 'NONE',  ( 28.00000000000001066, 65.75000000000001421, 75.00000000000000000 ) ) ;
#7233 = ORIENTED_EDGE ( 'NONE', *, *, #5912, .T. ) ;
#7234 = AXIS2_PLACEMENT_3D ( 'NONE', #4364, #18894, #20366 ) ;
#7235 = AXIS2_PLACEMENT_3D ( 'NONE', #8138, #19391, #12725 ) ;
#7236 = DIRECTION ( 'NONE',  ( -1.000000000000000000, 0.000000000000000000, 0.000000000000000000 ) ) ;
#7237 = LINE ( 'NONE', #20071, #8126 ) ;
#7238 = CARTESIAN_POINT ( 'NONE',  ( -15.99999999999999289, -10.00000000000000000, -5.999999999999989342 ) ) ;
#7239 = PLANE ( 'NONE',  #14195 ) ;
#7241 = EDGE_LOOP ( 'NONE', ( #6194, #11095, #12100, #17906 ) ) ;
#7240 = ORIENTED_EDGE ( 'NONE', *, *, #1948, .F. ) ;
#7242 = ORIENTED_EDGE ( 'NONE', *, *, #12591, .T. ) ;
#7243 = DIRECTION ( 'NONE',  ( -0.8660254037844370423, -0.5000000000000026645, 0.000000000000000000 ) ) ;
#7244 = CARTESIAN_POINT ( 'NONE',  ( 64.18022169236998309, 116.7929646387040918, 41.00000000000001421 ) ) ;
#7245 = CARTESIAN_POINT ( 'NONE',  ( -33.48481952675158624, 76.25000000000001421, -2.578432583507804132 ) ) ;
#7246 = CARTESIAN_POINT ( 'NONE',  ( 80.61604135543218774, 67.52081658169056766, -25.56477633425226159 ) ) ;
#7247 = EDGE_CURVE ( 'NONE', #4281, #456, #10269, .T. ) ;
#7248 = CARTESIAN_POINT ( 'NONE',  ( -29.99999999999999645, 4.999999999999999112, -0.9468725184748323365 ) ) ;
#7249 = CIRCLE ( 'NONE', #148, 12.47473710546057823 ) ;
#7250 = CARTESIAN_POINT ( 'NONE',  ( 49.86389338619021316, 127.5895726428436205, -12.50000000000000000 ) ) ;
#7251 = ORIENTED_EDGE ( 'NONE', *, *, #10984, .T. ) ;
#7252 = CARTESIAN_POINT ( 'NONE',  ( 78.40252712997106244, 56.59081475091886659, -22.42589158092872026 ) ) ;
#7253 = DIRECTION ( 'NONE',  ( -0.3878556453522130631, 0.6717856837524455171, 0.6310879443260485333 ) ) ;
#7254 = VERTEX_POINT ( 'NONE', #20041 ) ;
#7255 = CARTESIAN_POINT ( 'NONE',  ( 203.3234976231973405, 23.93187681866832861, -14.19648256269664621 ) ) ;
#7256 = CARTESIAN_POINT ( 'NONE',  ( 228.3428354930886428, 39.21401000532728887, -17.48830818005197330 ) ) ;
#7257 = CARTESIAN_POINT ( 'NONE',  ( -15.99999999999998934, 9.999999999999994671, 17.50000000000000000 ) ) ;
#7258 = CARTESIAN_POINT ( 'NONE',  ( 96.89297785063146762, 198.6243099879737599, 10.67381219715677609 ) ) ;
#7259 = FACE_OUTER_BOUND ( 'NONE', #1835, .T. ) ;
#7260 = ORIENTED_EDGE ( 'NONE', *, *, #7708, .T. ) ;
#7261 = ORIENTED_EDGE ( 'NONE', *, *, #2506, .F. ) ;
#7262 = DIRECTION ( 'NONE',  ( 0.8660254037844372643, 0.5000000000000027756, -0.000000000000000000 ) ) ;
#7263 = CARTESIAN_POINT ( 'NONE',  ( 5.000000000000000000, 0.000000000000000000, 0.000000000000000000 ) ) ;
#7264 = ORIENTED_EDGE ( 'NONE', *, *, #12783, .T. ) ;
#7265 = FILL_AREA_STYLE_COLOUR ( '', #6179 ) ;
#7266 = LINE ( 'NONE', #15675, #7825 ) ;
#7267 = CARTESIAN_POINT ( 'NONE',  ( -15.99999999999999289, 80.00000000000000000, 0.000000000000000000 ) ) ;
#7268 = CARTESIAN_POINT ( 'NONE',  ( 5.000000000000004441, -2.342598717236899830, 4.057500000000059615 ) ) ;
#7269 = EDGE_CURVE ( 'NONE', #3223, #10497, #2664, .T. ) ;
#7270 = CARTESIAN_POINT ( 'NONE',  ( 103.0338439448600951, 187.9562061502930135, 11.00000000000001066 ) ) ;
#7271 = FACE_OUTER_BOUND ( 'NONE', #157, .T. ) ;
#7272 = CIRCLE ( 'NONE', #12047, 11.94520687646042667 ) ;
#7273 = DIRECTION ( 'NONE',  ( -0.9294597282054694043, 0.3689235878121848722, 0.000000000000000000 ) ) ;
#7274 = CARTESIAN_POINT ( 'NONE',  ( -16.97782023378069383, 50.47616464312733342, -16.24942753911562932 ) ) ;
#7275 = CARTESIAN_POINT ( 'NONE',  ( 89.18111854763502322, 139.4901410505960087, 41.00000000000001421 ) ) ;
#7276 = PLANE ( 'NONE',  #18043 ) ;
#7277 = EDGE_CURVE ( 'NONE', #5590, #4064, #2315, .T. ) ;
#7278 = DIRECTION ( 'NONE',  ( -1.000000000000000000, -0.000000000000000000, -0.000000000000000000 ) ) ;
#7280 = VERTEX_POINT ( 'NONE', #5708 ) ;
#7279 = ORIENTED_EDGE ( 'NONE', *, *, #20794, .F. ) ;
#7281 = ORIENTED_EDGE ( 'NONE', *, *, #3785, .T. ) ;
#7282 = FACE_OUTER_BOUND ( 'NONE', #13044, .T. ) ;
#7283 =( REPRESENTATION_RELATIONSHIP ('NONE','NONE', #4634, #14136 ) REPRESENTATION_RELATIONSHIP_WITH_TRANSFORMATION ( #12954 )SHAPE_REPRESENTATION_RELATIONSHIP( ) );
#7284 = CARTESIAN_POINT ( 'NONE',  ( 58.68839529967456059, 85.41356074434793300, -13.73659394825620872 ) ) ;
#7285 = B_SPLINE_CURVE_WITH_KNOTS ( 'NONE', 3,
 ( #19679, #13232, #18104, #16723 ),
 .UNSPECIFIED., .F., .F.,
 ( 4, 4 ),
 ( 4.387428243836594897E-05, 0.0006098005047196312922 ),
 .UNSPECIFIED. ) ;
#7286 = ORIENTED_EDGE ( 'NONE', *, *, #8855, .F. ) ;
#7287 = ORIENTED_EDGE ( 'NONE', *, *, #16586, .F. ) ;
#7288 = VERTEX_POINT ( 'NONE', #20351 ) ;
#7289 = DIRECTION ( 'NONE',  ( -0.8660254037844357100, -0.5000000000000051070, 0.000000000000000000 ) ) ;
#7290 = DIRECTION ( 'NONE',  ( 0.000000000000000000, -0.5000000000000022204, -0.8660254037844372643 ) ) ;
#7291 = EDGE_CURVE ( 'NONE', #16434, #8493, #7723, .T. ) ;
#7292 = VERTEX_POINT ( 'NONE', #5505 ) ;
#7293 = CIRCLE ( 'NONE', #17811, 6.500000000000000000 ) ;
#7294 = VERTEX_POINT ( 'NONE', #7520 ) ;
#7295 = ADVANCED_FACE ( 'NONE', ( #10375 ), #16526, .F. ) ;
#7296 = CARTESIAN_POINT ( 'NONE',  ( -31.74999999999995737, 9.797174393178825657E-16, -8.000000000000000000 ) ) ;
#7297 = ORIENTED_EDGE ( 'NONE', *, *, #16016, .F. ) ;
#7298 = CONICAL_SURFACE ( 'NONE', #4258, 4.509097725792825528, 0.5235987755983015912 ) ;
#7299 = DIRECTION ( 'NONE',  ( -0.5000000000000051070, 0.8660254037844359321, -0.000000000000000000 ) ) ;
#7300 = DIRECTION ( 'NONE',  ( 5.951344303839691563E-17, 3.436010235862028595E-17, 1.000000000000000000 ) ) ;
#7301 = CARTESIAN_POINT ( 'NONE',  ( 209.6893306017078373, 12.35788975548706148, -12.44595276995722877 ) ) ;
#7302 = EDGE_CURVE ( 'NONE', #14525, #13175, #14229, .T. ) ;
#7303 = CARTESIAN_POINT ( 'NONE',  ( 4.000000000000000000, -1.759474945355379072, 3.047500000000001652 ) ) ;
#7304 = CARTESIAN_POINT ( 'NONE',  ( -28.09482755115952912, 75.66345017797092964, 3.167069675338890722 ) ) ;
#7305 = CYLINDRICAL_SURFACE ( 'NONE', #20736, 3.902363844300889451 ) ;
#7306 = CIRCLE ( 'NONE', #17807, 1.000000000000000888 ) ;
#7307 = CARTESIAN_POINT ( 'NONE',  ( -27.87934135416876913, 73.83089348061925250, 3.891407385552697384 ) ) ;
#7308 = PLANE ( 'NONE',  #9931 ) ;
#7309 = CARTESIAN_POINT ( 'NONE',  ( 72.49529059433406530, 198.3908428320658288, 11.00000000000001066 ) ) ;
#7310 = VECTOR ( 'NONE', #1341, 1000.000000000000114 ) ;
#7311 = ORIENTED_EDGE ( 'NONE', *, *, #919, .T. ) ;
#7312 = AXIS2_PLACEMENT_3D ( 'NONE', #11242, #16122, #19188 ) ;
#7314 = ADVANCED_FACE ( 'NONE', ( #12519 ), #16871, .F. ) ;
#7313 = CARTESIAN_POINT ( 'NONE',  ( 82.56388879349609056, 59.39730502837629444, -0.2907553109146409076 ) ) ;
#7315 = VERTEX_POINT ( 'NONE', #7833 ) ;
#7316 = CARTESIAN_POINT ( 'NONE',  ( 216.3683575532814416, 33.19538101841234834, -14.00000000000004441 ) ) ;
#7317 = EDGE_CURVE ( 'NONE', #279, #3078, #20659, .T. ) ;
#7318 = DIRECTION ( 'NONE',  ( 0.000000000000000000, 0.000000000000000000, 1.000000000000000000 ) ) ;
#7319 = AXIS2_PLACEMENT_3D ( 'NONE', #12459, #18917, #7975 ) ;
#7320 = CARTESIAN_POINT ( 'NONE',  ( 196.1523298472990007, 4.542298725908849200, -18.76170504960097318 ) ) ;
#7321 = VERTEX_POINT ( 'NONE', #1382 ) ;
#7322 = VECTOR ( 'NONE', #10204, 999.9999999999998863 ) ;
#7323 = SURFACE_SIDE_STYLE ('',( #13812 ) ) ;
#7324 = DIRECTION ( 'NONE',  ( 0.8660254037844380415, 0.5000000000000014433, 0.000000000000000000 ) ) ;
#7325 = FACE_OUTER_BOUND ( 'NONE', #4673, .T. ) ;
#7326 = DIRECTION ( 'NONE',  ( 0.000000000000000000, 1.000000000000000000, -1.117161918529055683E-15 ) ) ;
#7327 = EDGE_CURVE ( 'NONE', #681, #8656, #16832, .T. ) ;
#7328 = B_SPLINE_CURVE_WITH_KNOTS ( 'NONE', 3,
 ( #4479, #876, #17410, #5626 ),
 .UNSPECIFIED., .F., .F.,
 ( 4, 4 ),
 ( 0.001660622604225808112, 0.002660042459396035584 ),
 .UNSPECIFIED. ) ;
#7329 = EDGE_CURVE ( 'NONE', #15055, #4567, #19521, .T. ) ;
#7330 = CARTESIAN_POINT ( 'NONE',  ( 218.5491876009870680, 37.69061213431084667, -11.78314368930802303 ) ) ;
#7331 = DIRECTION ( 'NONE',  ( -0.5000000000000049960, 0.8660254037844357100, -0.000000000000000000 ) ) ;
#7332 = CARTESIAN_POINT ( 'NONE',  ( -11.09376927746295038, 15.76828681233661378, 0.9644763388355668265 ) ) ;
#7333 = VERTEX_POINT ( 'NONE', #9210 ) ;
#7335 = EDGE_CURVE ( 'NONE', #491, #3383, #20878, .T. ) ;
#7334 = DIRECTION ( 'NONE',  ( 0.000000000000000000, 0.000000000000000000, 1.000000000000000000 ) ) ;
#7336 = LINE ( 'NONE', #1105, #693 ) ;
#7337 = CONICAL_SURFACE ( 'NONE', #20552, 13.07248899748297433, 0.6693469023067423196 ) ;
#7338 = CARTESIAN_POINT ( 'NONE',  ( 190.1694833127194499, 64.25747545832879837, -14.00000000000006395 ) ) ;
#7339 = CARTESIAN_POINT ( 'NONE',  ( 226.9758196714467715, 41.58175086316159508, -17.77545290933958100 ) ) ;
#7341 = VERTEX_POINT ( 'NONE', #11026 ) ;
#7340 = EDGE_LOOP ( 'NONE', ( #10035, #8028 ) ) ;
#7342 = ORIENTED_EDGE ( 'NONE', *, *, #6654, .T. ) ;
#7343 = DIRECTION ( 'NONE',  ( 0.8660254037844372643, 0.5000000000000027756, -0.000000000000000000 ) ) ;
#7344 = ORIENTED_EDGE ( 'NONE', *, *, #7441, .F. ) ;
#7345 = CARTESIAN_POINT ( 'NONE',  ( -23.35826929781130801, 79.96309310684573290, -11.40240185268723394 ) ) ;
#7346 = EDGE_CURVE ( 'NONE', #12709, #14678, #18528, .T. ) ;
#7347 = DIRECTION ( 'NONE',  ( 0.1017280065263233557, -0.1761980758562880223, -0.9790840876823206917 ) ) ;
#7348 = ORIENTED_EDGE ( 'NONE', *, *, #8161, .T. ) ;
#7349 = CIRCLE ( 'NONE', #9049, 4.999999999999993783 ) ;
#7350 = DIRECTION ( 'NONE',  ( -0.000000000000000000, -1.000000000000000000, 1.117161918529055486E-15 ) ) ;
#7351 = CARTESIAN_POINT ( 'NONE',  ( 228.1017308963826622, 39.63161541676052479, -9.756613004592562532 ) ) ;
#7352 = VECTOR ( 'NONE', #11805, 1000.000000000000227 ) ;
#7353 = VERTEX_POINT ( 'NONE', #16121 ) ;
#7354 = DIRECTION ( 'NONE',  ( -0.7743856023693681534, 0.000000000000000000, -0.6327139470906508745 ) ) ;
#7355 = CARTESIAN_POINT ( 'NONE',  ( 207.0013954503587286, 3.383002205901548098, -25.76107385416581508 ) ) ;
#7356 = DIRECTION ( 'NONE',  ( 0.8660254037844378194, 0.5000000000000013323, 0.000000000000000000 ) ) ;
#7357 = DIRECTION ( 'NONE',  ( 0.8660254037844372643, 0.5000000000000027756, -0.000000000000000000 ) ) ;
#7358 = CARTESIAN_POINT ( 'NONE',  ( 219.8702716421484809, 33.88892106552722794, -17.38313153181864479 ) ) ;
#7359 = B_SPLINE_CURVE_WITH_KNOTS ( 'NONE', 3,
 ( #20858, #12622, #1069, #6331 ),
 .UNSPECIFIED., .F., .F.,
 ( 4, 4 ),
 ( 2.336863442359664515E-05, 0.0005892948567197438389 ),
 .UNSPECIFIED. ) ;
#7360 = ORIENTED_EDGE ( 'NONE', *, *, #12072, .T. ) ;
#7361 = EDGE_LOOP ( 'NONE', ( #9059, #5627, #19510, #6223, #216 ) ) ;
#7362 = DIRECTION ( 'NONE',  ( 0.5000000000000054401, -0.8660254037844354880, 0.000000000000000000 ) ) ;
#7363 = CARTESIAN_POINT ( 'NONE',  ( 10.40000000000000036, 0.000000000000000000, 0.000000000000000000 ) ) ;
#7364 = ORIENTED_EDGE ( 'NONE', *, *, #7329, .T. ) ;
#7365 = ORIENTED_EDGE ( 'NONE', *, *, #3990, .T. ) ;
#7366 = FACE_OUTER_BOUND ( 'NONE', #5045, .T. ) ;
#7367 = PRODUCT ( 'V-Trough Drill Bit Carrier Bed', 'V-Trough Drill Bit Carrier Bed', '', ( #5935 ) ) ;
#7368 = FACE_OUTER_BOUND ( 'NONE', #4459, .T. ) ;
#7369 = CARTESIAN_POINT ( 'NONE',  ( 193.9677224586705222, 21.99441912408888555, -14.00000000000005329 ) ) ;
#7370 = AXIS2_PLACEMENT_3D ( 'NONE', #5815, #15292, #13683 ) ;
#7371 = CARTESIAN_POINT ( 'NONE',  ( -35.00000000000000000, 65.74999999999997158, 1.479896280015810639 ) ) ;
#7372 = CARTESIAN_POINT ( 'NONE',  ( 208.0983737146324870, 5.661548828456886895, -14.00000000000005507 ) ) ;
#7373 = ORIENTED_EDGE ( 'NONE', *, *, #17861, .T. ) ;
#7374 = CARTESIAN_POINT ( 'NONE',  ( 208.0983737146324870, 5.661548828456886895, -14.00000000000005507 ) ) ;
#7375 = CIRCLE ( 'NONE', #10418, 2.961423854602166283 ) ;
#7376 = CARTESIAN_POINT ( 'NONE',  ( -14.51899950647152515, 49.50754942154606653, -12.41803798875660014 ) ) ;
#7377 = DIRECTION ( 'NONE',  ( 0.4999999999999995004, -0.8660254037844390407, 0.000000000000000000 ) ) ;
#7378 =( GEOMETRIC_REPRESENTATION_CONTEXT ( 3 ) GLOBAL_UNCERTAINTY_ASSIGNED_CONTEXT ( ( #20801 ) ) GLOBAL_UNIT_ASSIGNED_CONTEXT ( ( #20084, #5648, #15029 ) ) REPRESENTATION_CONTEXT ( 'NONE', 'WORKASPACE' ) );
#7379 = CARTESIAN_POINT ( 'NONE',  ( 218.1839418517603235, 38.32323632922017254, -14.53509620734043217 ) ) ;
#7380 = CARTESIAN_POINT ( 'NONE',  ( 220.5225658109747542, 32.75911442363913295, -10.52647298641115903 ) ) ;
#7381 = EDGE_CURVE ( 'NONE', #8117, #425, #9694, .T. ) ;
#7383 = ORIENTED_EDGE ( 'NONE', *, *, #6654, .F. ) ;
#7382 = ORIENTED_EDGE ( 'NONE', *, *, #16934, .F. ) ;
#7384 = CARTESIAN_POINT ( 'NONE',  ( 201.8742410413690322, 26.32933402587430294, -13.24682712576759158 ) ) ;
#7385 = CARTESIAN_POINT ( 'NONE',  ( 182.3972143829817867, 2.035126980567750099, -6.000000000000071942 ) ) ;
#7386 = DIRECTION ( 'NONE',  ( 0.4926956718456823592, -0.8533739363059945626, 0.1703053134172390071 ) ) ;
#7387 = ORIENTED_EDGE ( 'NONE', *, *, #2171, .F. ) ;
#7388 = ORIENTED_EDGE ( 'NONE', *, *, #10924, .F. ) ;
#7389 = ORIENTED_EDGE ( 'NONE', *, *, #14339, .T. ) ;
#7390 = CARTESIAN_POINT ( 'NONE',  ( 9.014528480800532151, 248.3427481158983596, 1.000000000000018208 ) ) ;
#7391 = CARTESIAN_POINT ( 'NONE',  ( -12.88155099176341878, 50.42675226781113196, -16.05345949917837345 ) ) ;
#7392 = DIRECTION ( 'NONE',  ( 1.000000000000000000, -0.000000000000000000, -0.000000000000000000 ) ) ;
#7393 = AXIS2_PLACEMENT_3D ( 'NONE', #20061, #13917, #14031 ) ;
#7394 = ORIENTED_EDGE ( 'NONE', *, *, #12518, .T. ) ;
#7395 = VERTEX_POINT ( 'NONE', #6235 ) ;
#7396 = CARTESIAN_POINT ( 'NONE',  ( 85.37797649651368204, 230.0773763115391262, 1.000000000000017097 ) ) ;
#7397 = CARTESIAN_POINT ( 'NONE',  ( -20.31374355284814825, 64.25000000000000000, -2.528164662410438357 ) ) ;
#7398 = CARTESIAN_POINT ( 'NONE',  ( 203.7831613941889088, 8.947961373646505123, -25.80036831778739881 ) ) ;
#7399 = FACE_OUTER_BOUND ( 'NONE', #4200, .T. ) ;
#7400 = CARTESIAN_POINT ( 'NONE',  ( 212.9607779367323417, 18.37065867240589156, -8.669480444820855780 ) ) ;
#7401 = DIRECTION ( 'NONE',  ( 0.000000000000000000, 0.000000000000000000, -1.000000000000000000 ) ) ;
#7402 = LINE ( 'NONE', #5704, #2780 ) ;
#7403 = DIRECTION ( 'NONE',  ( 0.5171545105027484102, 0.2985792958513954209, -0.8021231927550452889 ) ) ;
#7404 = CARTESIAN_POINT ( 'NONE',  ( 209.4102522745655506, 3.389308509292514149, -14.00000000000005507 ) ) ;
#7405 = APPLICATION_CONTEXT ( 'automotive_design' ) ;
#7406 = EDGE_CURVE ( 'NONE', #15178, #7292, #12724, .T. ) ;
#7407 = ORIENTED_EDGE ( 'NONE', *, *, #20343, .T. ) ;
#7408 = DIRECTION ( 'NONE',  ( 0.000000000000000000, 1.000000000000000000, -1.224646799147353207E-16 ) ) ;
#7409 = CARTESIAN_POINT ( 'NONE',  ( 5.000000000000000000, 2.342598717236900718, -4.057500000000001883 ) ) ;
#7410 = CYLINDRICAL_SURFACE ( 'NONE', #15666, 12.50000000000000000 ) ;
#7411 = AXIS2_PLACEMENT_3D ( 'NONE', #13366, #5079, #10368 ) ;
#7412 = ADVANCED_FACE ( 'NONE', ( #18879 ), #9308, .F. ) ;
#7413 = ORIENTED_EDGE ( 'NONE', *, *, #15108, .T. ) ;
#7414 = CARTESIAN_POINT ( 'NONE',  ( 82.68772507326825405, 59.96207871578241821, -0.1148040406626176790 ) ) ;
#7415 = ORIENTED_EDGE ( 'NONE', *, *, #14357, .F. ) ;
#7416 = ORIENTED_EDGE ( 'NONE', *, *, #11156, .T. ) ;
#7417 = PLANE ( 'NONE',  #18971 ) ;
#7418 = CARTESIAN_POINT ( 'NONE',  ( 196.8817620068315080, 4.786426675387034813, -7.327415643059290495 ) ) ;
#7419 = VECTOR ( 'NONE', #17945, 1000.000000000000227 ) ;
#7420 = EDGE_CURVE ( 'NONE', #14942, #14915, #7004, .T. ) ;
#7421 = APPLICATION_PROTOCOL_DEFINITION ( 'draft international standard', 'automotive_design', 1998, #17457 ) ;
#7422 = DIRECTION ( 'NONE',  ( -0.1997192025788214198, -0.1153079353712215815, -0.9730448705798235842 ) ) ;
#7423 = VERTEX_POINT ( 'NONE', #19187 ) ;
#7424 = CARTESIAN_POINT ( 'NONE',  ( 226.3048421647687860, 42.74391799546372539, -11.31761084191175470 ) ) ;
#7425 = FACE_OUTER_BOUND ( 'NONE', #4894, .T. ) ;
#7426 = FACE_OUTER_BOUND ( 'NONE', #14573, .T. ) ;
#7427 = CARTESIAN_POINT ( 'NONE',  ( 221.5400775418029298, 33.12808716631536043, -11.12998660979008569 ) ) ;
#7428 = EDGE_CURVE ( 'NONE', #12664, #1475, #4659, .T. ) ;
#7429 = AXIS2_PLACEMENT_3D ( 'NONE', #1666, #8005, #12910 ) ;
#7430 = CARTESIAN_POINT ( 'NONE',  ( 209.9266392777186923, 12.49489998346296460, -14.00000000000005507 ) ) ;
#7431 = ADVANCED_FACE ( 'NONE', ( #8350 ), #4962, .F. ) ;
#7432 = FACE_OUTER_BOUND ( 'NONE', #2723, .T. ) ;
#7433 = CARTESIAN_POINT ( 'NONE',  ( 210.7598317367304332, 3.058394523489540884, -14.00000000000005507 ) ) ;
#7434 = CARTESIAN_POINT ( 'NONE',  ( 205.6843207647078771, 2.880188005405192264, -2.388950188371906869 ) ) ;
#7435 = ORIENTED_EDGE ( 'NONE', *, *, #5992, .T. ) ;
#7436 = FACE_OUTER_BOUND ( 'NONE', #5898, .T. ) ;
#7437 = CARTESIAN_POINT ( 'NONE',  ( -3.510843195177425713, 80.00000000000000000, 0.5205403966592460074 ) ) ;
#7438 = LINE ( 'NONE', #2696, #9859 ) ;
#7439 = AXIS2_PLACEMENT_3D ( 'NONE', #6593, #17963, #3431 ) ;
#7440 = CARTESIAN_POINT ( 'NONE',  ( 61.47152125231750830, 217.4845714233581475, 45.12705109663956193 ) ) ;
#7441 = EDGE_CURVE ( 'NONE', #8757, #10193, #14854, .T. ) ;
#7443 = ORIENTED_EDGE ( 'NONE', *, *, #19352, .T. ) ;
#7442 = ORIENTED_EDGE ( 'NONE', *, *, #6809, .F. ) ;
#7444 = ORIENTED_EDGE ( 'NONE', *, *, #14255, .F. ) ;
#7445 = CIRCLE ( 'NONE', #10482, 12.47473710546057823 ) ;
#7446 = ORIENTED_EDGE ( 'NONE', *, *, #2558, .F. ) ;
#7447 = ADVANCED_FACE ( 'NONE', ( #17915 ), #6437, .T. ) ;
#7448 = DIRECTION ( 'NONE',  ( 0.8660254037844370423, 0.5000000000000026645, -0.000000000000000000 ) ) ;
#7449 = ORIENTED_EDGE ( 'NONE', *, *, #4244, .T. ) ;
#7450 = VECTOR ( 'NONE', #20360, 1000.000000000000227 ) ;
#7451 = CARTESIAN_POINT ( 'NONE',  ( -34.33329038210762718, 64.25000000000000000, -2.193932927905879904 ) ) ;
#7452 = CARTESIAN_POINT ( 'NONE',  ( 227.9553588074475670, 39.88513931160575510, -14.00000000000005507 ) ) ;
#7453 = AXIS2_PLACEMENT_3D ( 'NONE', #16425, #1902, #11971 ) ;
#7454 =( NAMED_UNIT ( * ) PLANE_ANGLE_UNIT ( ) SI_UNIT ( $, .RADIAN. ) );
#7455 = CARTESIAN_POINT ( 'NONE',  ( 195.7326308045045380, 3.945958789216395424, -9.783550055872323625 ) ) ;
#7456 = EDGE_CURVE ( 'NONE', #3353, #2978, #6346, .T. ) ;
#7457 = AXIS2_PLACEMENT_3D ( 'NONE', #9750, #11359, #543 ) ;
#7458 = FACE_OUTER_BOUND ( 'NONE', #11503, .T. ) ;
#7459 = AXIS2_PLACEMENT_3D ( 'NONE', #6108, #19066, #16001 ) ;
#7460 = CARTESIAN_POINT ( 'NONE',  ( 0.000000000000000000, 0.000000000000000000, 0.000000000000000000 ) ) ;
#7461 = CIRCLE ( 'NONE', #14609, 3.902363844300875240 ) ;
#7462 = ORIENTED_EDGE ( 'NONE', *, *, #18872, .F. ) ;
#7463 = DIRECTION ( 'NONE',  ( 0.6946590618905412740, 0.4010615963775223669, -0.5971585917027958379 ) ) ;
#7464 = LINE ( 'NONE', #12364, #17868 ) ;
#7465 = EDGE_CURVE ( 'NONE', #13435, #13758, #11759, .T. ) ;
#7466 = CARTESIAN_POINT ( 'NONE',  ( 227.9152326730940672, 38.97517392395430846, -10.17395310825082611 ) ) ;
#7467 = FACE_OUTER_BOUND ( 'NONE', #1833, .T. ) ;
#7468 = PLANE ( 'NONE',  #3268 ) ;
#7470 = EDGE_LOOP ( 'NONE', ( #8545, #1058, #1501, #2052, #4841 ) ) ;
#7469 = ORIENTED_EDGE ( 'NONE', *, *, #16379, .F. ) ;
#7471 = VERTEX_POINT ( 'NONE', #5165 ) ;
#7472 = DIRECTION ( 'NONE',  ( 0.000000000000000000, 0.000000000000000000, -1.000000000000000000 ) ) ;
#7473 = EDGE_CURVE ( 'NONE', #950, #14788, #18765, .T. ) ;
#7474 = CIRCLE ( 'NONE', #1064, 3.902363844300875240 ) ;
#7475 = ORIENTED_EDGE ( 'NONE', *, *, #5888, .F. ) ;
#7476 = ORIENTED_EDGE ( 'NONE', *, *, #7335, .T. ) ;
#7477 = CARTESIAN_POINT ( 'NONE',  ( 217.9607779367323985, 9.710404634561534465, -8.669480444820854004 ) ) ;
#7478 = DIRECTION ( 'NONE',  ( -0.5000000000000005551, 0.8660254037844382635, 0.000000000000000000 ) ) ;
#7479 = VECTOR ( 'NONE', #7863, 999.9999999999998863 ) ;
#7480 = VECTOR ( 'NONE', #2302, 1000.000000000000114 ) ;
#7481 = LINE ( 'NONE', #9373, #15138 ) ;
#7482 = ADVANCED_FACE ( 'NONE', ( #6750 ), #9730, .F. ) ;
#7483 = AXIS2_PLACEMENT_3D ( 'NONE', #18172, #15017, #13511 ) ;
#7484 = DIRECTION ( 'NONE',  ( 0.8660254037844355990, 0.5000000000000054401, 0.000000000000000000 ) ) ;
#7485 = DIRECTION ( 'NONE',  ( -1.000000000000000000, -0.000000000000000000, -0.000000000000000000 ) ) ;
#7486 = AXIS2_PLACEMENT_3D ( 'NONE', #18003, #8120, #1676 ) ;
#7487 = EDGE_LOOP ( 'NONE', ( #13412, #8887, #9081, #11780 ) ) ;
#7488 = CARTESIAN_POINT ( 'NONE',  ( 221.7236785435837021, 32.19223253356614123, -13.56204498775467293 ) ) ;
#7489 = AXIS2_PLACEMENT_3D ( 'NONE', #9245, #18807, #2702 ) ;
#7490 = CARTESIAN_POINT ( 'NONE',  ( -12.17658180577358173, 50.40238676466552192, -15.95319627043026856 ) ) ;
#7491 = DIRECTION ( 'NONE',  ( 0.5000000000000054401, -0.8660254037844354880, 0.000000000000000000 ) ) ;
#7492 = VECTOR ( 'NONE', #16866, 1000.000000000000000 ) ;
#7493 = VECTOR ( 'NONE', #5221, 1000.000000000000000 ) ;
#7494 = CARTESIAN_POINT ( 'NONE',  ( 214.9776847560361830, 7.988114983668789471, -4.409371045253012156 ) ) ;
#7495 = VECTOR ( 'NONE', #2868, 999.9999999999998863 ) ;
#7496 = PLANE ( 'NONE',  #4936 ) ;
#7498 = ORIENTED_EDGE ( 'NONE', *, *, #8083, .T. ) ;
#7497 = ORIENTED_EDGE ( 'NONE', *, *, #4342, .F. ) ;
#7499 = CARTESIAN_POINT ( 'NONE',  ( 204.9818247258934321, 9.640009970873835599, -14.00000000000005507 ) ) ;
#7500 = PLANE ( 'NONE',  #7808 ) ;
#7501 = CARTESIAN_POINT ( 'NONE',  ( 226.7278977660763246, 42.01116419957243409, -10.52647298641110751 ) ) ;
#7502 = ORIENTED_EDGE ( 'NONE', *, *, #10960, .F. ) ;
#7503 = DIRECTION ( 'NONE',  ( -0.8660254037844360431, -0.5000000000000045519, -0.000000000000000000 ) ) ;
#7504 = LINE ( 'NONE', #2646, #5415 ) ;
#7505 = CARTESIAN_POINT ( 'NONE',  ( -31.93034077464222165, 50.51989448544605921, -8.569845794639380898 ) ) ;
#7506 = CARTESIAN_POINT ( 'NONE',  ( -34.66662763442661799, 65.74999999999997158, -1.859747928060476729 ) ) ;
#7507 = ORIENTED_EDGE ( 'NONE', *, *, #5219, .T. ) ;
#7508 = ORIENTED_EDGE ( 'NONE', *, *, #5523, .T. ) ;
#7509 = DIRECTION ( 'NONE',  ( 0.8660254037844368202, 0.5000000000000031086, 0.000000000000000000 ) ) ;
#7510 = VECTOR ( 'NONE', #7774, 1000.000000000000227 ) ;
#7511 = DIRECTION ( 'NONE',  ( -0.5000000000000051070, 0.8660254037844359321, -0.000000000000000000 ) ) ;
#7512 = CIRCLE ( 'NONE', #1443, 3.619616396367202782 ) ;
#7513 = DIRECTION ( 'NONE',  ( -0.7377723590286303645, 0.4392898442850237672, 0.5125586590443765855 ) ) ;
#7514 = B_SPLINE_CURVE_WITH_KNOTS ( 'NONE', 3,
 ( #1453, #11092, #11198, #14301 ),
 .UNSPECIFIED., .F., .F.,
 ( 4, 4 ),
 ( 3.280426939088333109E-07, 0.0006729788347424356214 ),
 .UNSPECIFIED. ) ;
#7515 = EDGE_CURVE ( 'NONE', #7969, #6373, #9448, .T. ) ;
#7516 = CARTESIAN_POINT ( 'NONE',  ( -15.67065502568128288, 20.09941697557067997, 12.49999999999999822 ) ) ;
#7517 = CARTESIAN_POINT ( 'NONE',  ( 227.5312376355471145, 39.64027283883993391, -14.00000000000005507 ) ) ;
#7518 = DIRECTION ( 'NONE',  ( -0.5000000000000054401, 0.8660254037844354880, -0.000000000000000000 ) ) ;
#7519 = CARTESIAN_POINT ( 'NONE',  ( 63.15554463217812042, 234.5677573683057062, -14.00000000000003020 ) ) ;
#7520 = CARTESIAN_POINT ( 'NONE',  ( 34.99529059433363898, 263.3427481158985302, -22.00000000000000355 ) ) ;
#7521 = DIRECTION ( 'NONE',  ( -0.1017280065263233557, 0.1761980758562880223, 0.9790840876823206917 ) ) ;
#7522 = CARTESIAN_POINT ( 'NONE',  ( -29.99999999999999645, 5.000000000000000000, -15.00000000000000000 ) ) ;
#7523 = EDGE_LOOP ( 'NONE', ( #2810, #8231, #1992, #10522, #14786 ) ) ;
#7524 = AXIS2_PLACEMENT_3D ( 'NONE', #16993, #13060, #14561 ) ;
#7525 = CARTESIAN_POINT ( 'NONE',  ( 82.70822966583139646, 64.11489447924186891, 0.5923196681384729212 ) ) ;
#7526 = ADVANCED_FACE ( 'NONE', ( #110 ), #2003, .F. ) ;
#7527 = CONICAL_SURFACE ( 'NONE', #18375, 38.65920715899539317, 0.03863996524032856789 ) ;
#7528 = ORIENTED_EDGE ( 'NONE', *, *, #10029, .T. ) ;
#7529 = VERTEX_POINT ( 'NONE', #3487 ) ;
#7530 = CARTESIAN_POINT ( 'NONE',  ( 1.312845613648171650, 74.81579058300722807, -1.112382790403132926 ) ) ;
#7531 = DIRECTION ( 'NONE',  ( 0.8660254037844370423, 0.5000000000000026645, -0.000000000000000000 ) ) ;
#7532 = B_SPLINE_CURVE_WITH_KNOTS ( 'NONE', 3,
 ( #5713, #20250, #10166, #3712, #8596, #13698, #13902, #5510, #20147, #2565, #12099, #2459, #8808, #3825 ),
 .UNSPECIFIED., .F., .F.,
 ( 4, 2, 2, 2, 2, 2, 4 ),
 ( 0.000000000000000000, 0.001404842194932280066, 0.002107263292398419557, 0.002809684389864558832, 0.003512105487330698540, 0.004214526584796837380, 0.005619368779729116796 ),
 .UNSPECIFIED. ) ;
#7533 = PRODUCT_CONTEXT ( 'NONE', #20702, 'mechanical' ) ;
#7534 = ADVANCED_FACE ( 'NONE', ( #8451 ), #16628, .F. ) ;
#7535 = LINE ( 'NONE', #14027, #2849 ) ;
#7536 = EDGE_LOOP ( 'NONE', ( #1452, #8223, #9526, #10707, #5451, #12166 ) ) ;
#7537 = EDGE_CURVE ( 'NONE', #1461, #16239, #13548, .T. ) ;
#7538 = CARTESIAN_POINT ( 'NONE',  ( 229.1807915133727249, 37.76262760368712179, -17.47639052459127385 ) ) ;
#7539 = CIRCLE ( 'NONE', #13305, 8.000000000000058620 ) ;
#7540 = LINE ( 'NONE', #20159, #16781 ) ;
#7541 = DIRECTION ( 'NONE',  ( -0.5000000000000049960, 0.8660254037844357100, -0.000000000000000000 ) ) ;
#7542 = LINE ( 'NONE', #5730, #5140 ) ;
#7543 = DIRECTION ( 'NONE',  ( -1.000000000000000000, -0.000000000000000000, -0.000000000000000000 ) ) ;
#7544 = CARTESIAN_POINT ( 'NONE',  ( 218.7199378970581733, 35.88135755768452384, -17.38313153181858084 ) ) ;
#7545 = LINE ( 'NONE', #14038, #6005 ) ;
#7546 = ORIENTED_EDGE ( 'NONE', *, *, #18466, .T. ) ;
#7547 = CARTESIAN_POINT ( 'NONE',  ( 212.8532021079397225, 7.019143578708644249, -2.867675856073738760 ) ) ;
#7548 = CARTESIAN_POINT ( 'NONE',  ( 209.3577481411911663, 3.480248335904243095, -14.00000000000005507 ) ) ;
#7549 = ADVANCED_BREP_SHAPE_REPRESENTATION ( '', ( #17843, #18233 ), #3328 ) ;
#7550 = DIRECTION ( 'NONE',  ( 0.8660254037844374864, 0.5000000000000021094, 6.938893903907228378E-16 ) ) ;
#7551 = CYLINDRICAL_SURFACE ( 'NONE', #17567, 4.999999999999975131 ) ;
#7552 = VECTOR ( 'NONE', #20474, 1000.000000000000000 ) ;
#7553 = B_SPLINE_CURVE_WITH_KNOTS ( 'NONE', 3,
 ( #3995, #2102, #18203, #511 ),
 .UNSPECIFIED., .F., .F.,
 ( 4, 4 ),
 ( 1.840348241542355323E-05, 0.0005843297047112946041 ),
 .UNSPECIFIED. ) ;
#7555 = ORIENTED_EDGE ( 'NONE', *, *, #5788, .T. ) ;
#7554 = ORIENTED_EDGE ( 'NONE', *, *, #2178, .T. ) ;
#7556 = DIRECTION ( 'NONE',  ( -0.000000000000000000, 0.8660254037844394848, 0.4999999999999985012 ) ) ;
#7557 = DIRECTION ( 'NONE',  ( 0.5000000000000057732, -0.8660254037844352659, -1.942890293094023699E-16 ) ) ;
#7558 = EDGE_LOOP ( 'NONE', ( #14179, #13784, #15434, #19801 ) ) ;
#7559 = EDGE_CURVE ( 'NONE', #13544, #19831, #14750, .T. ) ;
#7560 = CARTESIAN_POINT ( 'NONE',  ( 221.4960551238412734, 32.55646305549218056, -12.27491058351084519 ) ) ;
#7561 = CYLINDRICAL_SURFACE ( 'NONE', #10400, 3.902363844300889451 ) ;
#7562 = ADVANCED_FACE ( 'NONE', ( #14955 ), #18218, .T. ) ;
#7563 = CARTESIAN_POINT ( 'NONE',  ( -35.00000000000000000, 65.74999999999997158, 1.479896280015810639 ) ) ;
#7564 = DIRECTION ( 'NONE',  ( 0.5000000000000043299, -0.8660254037844361541, -1.224510688924805588E-16 ) ) ;
#7565 = AXIS2_PLACEMENT_3D ( 'NONE', #13891, #18658, #15397 ) ;
#7566 =( REPRESENTATION_RELATIONSHIP ('NONE','NONE', #4634, #20473 ) REPRESENTATION_RELATIONSHIP_WITH_TRANSFORMATION ( #14241 )SHAPE_REPRESENTATION_RELATIONSHIP( ) );
#7567 = VECTOR ( 'NONE', #8480, 1000.000000000000114 ) ;
#7568 = CARTESIAN_POINT ( 'NONE',  ( 0.000000000000000000, 0.000000000000000000, 0.000000000000000000 ) ) ;
#7569 = ADVANCED_FACE ( 'NONE', ( #10134 ), #6644, .T. ) ;
#7570 = ORIENTED_EDGE ( 'NONE', *, *, #12917, .F. ) ;
#7571 = DIRECTION ( 'NONE',  ( 0.5000000000000051070, -0.8660254037844359321, 0.000000000000000000 ) ) ;
#7572 = CARTESIAN_POINT ( 'NONE',  ( 22.00490953756706958, 255.8427481158984165, -28.99999999999997513 ) ) ;
#7573 = DIRECTION ( 'NONE',  ( 0.5000000000000049960, -0.8660254037844358210, 0.000000000000000000 ) ) ;
#7574 = DIRECTION ( 'NONE',  ( 0.8660254037844377084, 0.5000000000000017764, 0.000000000000000000 ) ) ;
#7575 = DIRECTION ( 'NONE',  ( 0.000000000000000000, 0.000000000000000000, 1.000000000000000000 ) ) ;
#7576 = ORIENTED_EDGE ( 'NONE', *, *, #14862, .T. ) ;
#7577 = ORIENTED_EDGE ( 'NONE', *, *, #12093, .F. ) ;
#7578 = FACE_BOUND ( 'NONE', #966, .T. ) ;
#7579 = ADVANCED_FACE ( 'NONE', ( #8030 ), #18016, .T. ) ;
#7580 = ORIENTED_EDGE ( 'NONE', *, *, #11443, .F. ) ;
#7581 = VERTEX_POINT ( 'NONE', #16838 ) ;
#7582 = LINE ( 'NONE', #9371, #4453 ) ;
#7583 = DIRECTION ( 'NONE',  ( 0.3841106397986906451, -0.6652991438591134843, 0.6401843996644803747 ) ) ;
#7584 = FACE_OUTER_BOUND ( 'NONE', #4534, .T. ) ;
#7585 = VECTOR ( 'NONE', #14221, 1000.000000000000227 ) ;
#7586 = EDGE_CURVE ( 'NONE', #8365, #9396, #12173, .T. ) ;
#7587 = CARTESIAN_POINT ( 'NONE',  ( 5.000000000000000000, 7.027796151710712813, -4.057500000000007212 ) ) ;
#7588 = CARTESIAN_POINT ( 'NONE',  ( 200.8946500511725333, -0.1427288941911568354, -6.310089745291766583 ) ) ;
#7589 = VERTEX_POINT ( 'NONE', #10351 ) ;
#7590 = CARTESIAN_POINT ( 'NONE',  ( 217.1883462137477920, 38.53415216962800116, -14.58164069302991095 ) ) ;
#7591 = ADVANCED_FACE ( 'NONE', ( #4005 ), #522, .F. ) ;
#7592 = B_SPLINE_CURVE_WITH_KNOTS ( 'NONE', 3,
 ( #15080, #15183, #5178, #19597 ),
 .UNSPECIFIED., .F., .F.,
 ( 4, 4 ),
 ( 5.109387134629360757E-05, 0.0009050796093292725166 ),
 .UNSPECIFIED. ) ;
#7593 = EDGE_CURVE ( 'NONE', #11291, #19778, #9148, .T. ) ;
#7594 = CARTESIAN_POINT ( 'NONE',  ( -29.99999999999999645, 5.000000000000000000, -10.50000000000000178 ) ) ;
#7595 = CARTESIAN_POINT ( 'NONE',  ( -24.72758442336008855, 44.98735168799644413, -8.975511724720679041 ) ) ;
#7596 = DIRECTION ( 'NONE',  ( -0.8660254037844380415, -0.5000000000000014433, -0.000000000000000000 ) ) ;
#7597 = B_SPLINE_CURVE_WITH_KNOTS ( 'NONE', 3,
 ( #12759, #7968, #20797, #20895, #15841, #17424 ),
 .UNSPECIFIED., .F., .F.,
 ( 4, 2, 4 ),
 ( 0.001660622604225808112, 0.002656748863554461021, 0.003652875122883114146 ),
 .UNSPECIFIED. ) ;
#7598 = CARTESIAN_POINT ( 'NONE',  ( 0.000000000000000000, 3.518949890710767026, -4.987329993433320396E-15 ) ) ;
#7599 =( BOUNDED_CURVE ( )  B_SPLINE_CURVE ( 3, ( #14663, #6875, #16433, #10045 ),
 .UNSPECIFIED., .F., .T. ) 
 B_SPLINE_CURVE_WITH_KNOTS ( ( 4, 4 ),
 ( 3.141592653589790451, 4.712388980384689674 ),
 .UNSPECIFIED. ) 
 CURVE ( )  GEOMETRIC_REPRESENTATION_ITEM ( )  RATIONAL_B_SPLINE_CURVE ( ( 1.000000000000000000, 0.8047378541243643824, 0.8047378541243643824, 1.000000000000000000 ) ) 
 REPRESENTATION_ITEM ( '' )  );
#7600 = CARTESIAN_POINT ( 'NONE',  ( -28.07131995261575241, 46.63343660265383051, -3.263164565673607243 ) ) ;
#7602 = ORIENTED_EDGE ( 'NONE', *, *, #19091, .T. ) ;
#7601 = ORIENTED_EDGE ( 'NONE', *, *, #6263, .F. ) ;
#7603 = ORIENTED_EDGE ( 'NONE', *, *, #13824, .T. ) ;
#7604 = LINE ( 'NONE', #6003, #17983 ) ;
#7605 = DIRECTION ( 'NONE',  ( 0.8660254037844371533, 0.5000000000000025535, 7.216449660063516527E-16 ) ) ;
#7606 = EDGE_CURVE ( 'NONE', #15581, #8339, #19905, .T. ) ;
#7607 = DIRECTION ( 'NONE',  ( 0.8660254037844370423, 0.5000000000000026645, -0.000000000000000000 ) ) ;
#7608 = ORIENTED_EDGE ( 'NONE', *, *, #17135, .T. ) ;
#7609 = ORIENTED_EDGE ( 'NONE', *, *, #13714, .F. ) ;
#7610 = ORIENTED_EDGE ( 'NONE', *, *, #19445, .F. ) ;
#7611 = CARTESIAN_POINT ( 'NONE',  ( 30.10683012259193703, -24.14213562373095456, 4.999999999999997335 ) ) ;
#7612 = FACE_OUTER_BOUND ( 'NONE', #12837, .T. ) ;
#7613 = CARTESIAN_POINT ( 'NONE',  ( -33.12309443379005813, 51.54550291367893067, -5.857582128031854296 ) ) ;
#7614 = CARTESIAN_POINT ( 'NONE',  ( -27.65265446014365125, 9.445465779080201685, 4.571190765816516510 ) ) ;
#7615 = ORIENTED_EDGE ( 'NONE', *, *, #14555, .F. ) ;
#7616 = ORIENTED_EDGE ( 'NONE', *, *, #13154, .F. ) ;
#7617 = DIRECTION ( 'NONE',  ( 0.000000000000000000, 0.000000000000000000, -1.000000000000000000 ) ) ;
#7618 = ADVANCED_FACE ( 'NONE', ( #2322 ), #7276, .T. ) ;
#7619 = DIRECTION ( 'NONE',  ( -0.8296432542242749841, -0.4789947561577487245, 0.2868032327110942581 ) ) ;
#7620 = CARTESIAN_POINT ( 'NONE',  ( 61.57468973143931379, 78.66722686282992072, -24.21353532798446651 ) ) ;
#7621 = CONICAL_SURFACE ( 'NONE', #14074, 4.509097725792825528, 0.5235987755983015912 ) ;
#7622 = CARTESIAN_POINT ( 'NONE',  ( 227.9553588074475670, 39.88513931160575510, -14.00000000000005507 ) ) ;
#7623 = CARTESIAN_POINT ( 'NONE',  ( 211.9531851547456540, 13.48791688690614521, -4.253719131806259490 ) ) ;
#7624 = CARTESIAN_POINT ( 'NONE',  ( 107.3639709637822648, 190.4562061502930135, 11.00000000000001066 ) ) ;
#7625 = CARTESIAN_POINT ( 'NONE',  ( -15.99999999999999289, -10.00000000000000000, 5.999999999999989342 ) ) ;
#7626 = DIRECTION ( 'NONE',  ( -0.4999999999999995004, 0.8660254037844390407, 0.000000000000000000 ) ) ;
#7627 = DIRECTION ( 'NONE',  ( 0.8660254037844373753, 0.5000000000000022204, -6.661338147750940229E-16 ) ) ;
#7628 = CARTESIAN_POINT ( 'NONE',  ( 202.2239086947344617, 1.139925180369061097, -4.138477629886050835 ) ) ;
#7629 = DIRECTION ( 'NONE',  ( -0.5000000000000047740, 0.8660254037844358210, 0.000000000000000000 ) ) ;
#7630 = ORIENTED_EDGE ( 'NONE', *, *, #208, .T. ) ;
#7631 = VECTOR ( 'NONE', #1993, 1000.000000000000000 ) ;
#7632 = CARTESIAN_POINT ( 'NONE',  ( 80.83364148849122444, 66.21898444903385439, 0.4528609240599802965 ) ) ;
#7633 = VERTEX_POINT ( 'NONE', #7184 ) ;
#7634 = AXIS2_PLACEMENT_3D ( 'NONE', #3503, #10053, #8586 ) ;
#7635 = B_SPLINE_CURVE_WITH_KNOTS ( 'NONE', 3,
 ( #20761, #20654, #19083, #9414 ),
 .UNSPECIFIED., .F., .F.,
 ( 4, 4 ),
 ( 5.849083918475469174E-06, 0.0005717753062012811884 ),
 .UNSPECIFIED. ) ;
#7636 = ORIENTED_EDGE ( 'NONE', *, *, #18062, .F. ) ;
#7637 = CARTESIAN_POINT ( 'NONE',  ( -3.376929201035541617, 76.35052269458219598, -2.692414605357459134 ) ) ;
#7638 = VECTOR ( 'NONE', #15191, 1000.000000000000000 ) ;
#7639 = CARTESIAN_POINT ( 'NONE',  ( -15.99999999999999289, 10.09941697557069418, 4.999999999999989342 ) ) ;
#7640 = ITEM_DEFINED_TRANSFORMATION ( 'NONE', 'NONE', #5008,  #18233 ) ;
#7641 = CARTESIAN_POINT ( 'NONE',  ( 22.00490953756706958, 255.8427481158984165, 1.000000000000018208 ) ) ;
#7642 = ORIENTED_EDGE ( 'NONE', *, *, #2394, .T. ) ;
#7643 = FACE_OUTER_BOUND ( 'NONE', #12492, .T. ) ;
#7644 = DIRECTION ( 'NONE',  ( -0.5000000000000049960, 0.8660254037844358210, -0.000000000000000000 ) ) ;
#7645 = DIRECTION ( 'NONE',  ( 0.8660254037844360431, 0.5000000000000045519, 0.000000000000000000 ) ) ;
#7646 = CARTESIAN_POINT ( 'NONE',  ( 29.50490953756713353, 242.8523670591319785, -19.00000000000000355 ) ) ;
#7647 = AXIS2_PLACEMENT_3D ( 'NONE', #4667, #12841, #11137 ) ;
#7648 = CARTESIAN_POINT ( 'NONE',  ( 0.000000000000000000, 4.685197434473814759, -6.938893903907228378E-15 ) ) ;
#7649 = AXIS2_PLACEMENT_3D ( 'NONE', #5268, #16630, #3587 ) ;
#7650 = DIRECTION ( 'NONE',  ( 0.6123724356957944703, 0.3535533905932780607, -0.7071067811865454633 ) ) ;
#7651 = DIRECTION ( 'NONE',  ( 0.5000000000000051070, -0.8660254037844359321, 0.000000000000000000 ) ) ;
#7652 = CARTESIAN_POINT ( 'NONE',  ( 227.9553588074475954, 39.88513931160571957, -14.00000000000005507 ) ) ;
#7653 = VERTEX_POINT ( 'NONE', #2215 ) ;
#7654 = DIRECTION ( 'NONE',  ( -0.8660254037844362651, -0.5000000000000042188, 0.000000000000000000 ) ) ;
#7655 = LINE ( 'NONE', #20381, #2747 ) ;
#7656 = EDGE_CURVE ( 'NONE', #20210, #17471, #12687, .T. ) ;
#7657 = CIRCLE ( 'NONE', #3939, 5.000000000000001776 ) ;
#7658 = DIRECTION ( 'NONE',  ( 1.000000000000000000, -0.000000000000000000, -0.000000000000000000 ) ) ;
#7659 = PLANE ( 'NONE',  #6363 ) ;
#7661 = ORIENTED_EDGE ( 'NONE', *, *, #7148, .T. ) ;
#7660 = EDGE_LOOP ( 'NONE', ( #20749, #18221, #10464, #20438 ) ) ;
#7662 = CIRCLE ( 'NONE', #19502, 1.000000000000000888 ) ;
#7663 = CARTESIAN_POINT ( 'NONE',  ( -11.66624079247173995, 12.58454993689042034, 11.72627446870071388 ) ) ;
#7664 = CARTESIAN_POINT ( 'NONE',  ( 82.49529059433407951, 181.0703347563770365, 6.000000000000009770 ) ) ;
#7665 = ORIENTED_EDGE ( 'NONE', *, *, #14255, .T. ) ;
#7666 = CARTESIAN_POINT ( 'NONE',  ( 64.92628429094538944, 80.60227088397526529, -21.04771496906974448 ) ) ;
#7667 = VERTEX_POINT ( 'NONE', #18746 ) ;
#7668 = CARTESIAN_POINT ( 'NONE',  ( 227.5312376355471145, 39.64027283883993391, -14.00000000000005507 ) ) ;
#7669 = CARTESIAN_POINT ( 'NONE',  ( 218.7874248973968179, 10.18766947982593862, -16.70797078425240301 ) ) ;
#7670 = ADVANCED_FACE ( 'NONE', ( #10667 ), #3793, .T. ) ;
#7671 = DIRECTION ( 'NONE',  ( 0.5000000000000043299, -0.8660254037844361541, -1.224510688924805588E-16 ) ) ;
#7672 = ORIENTED_EDGE ( 'NONE', *, *, #1852, .F. ) ;
#7673 = CARTESIAN_POINT ( 'NONE',  ( 220.2180084519553134, 35.41797800104779270, -14.00000000000005507 ) ) ;
#7674 = VECTOR ( 'NONE', #13258, 1000.000000000000227 ) ;
#7675 = CARTESIAN_POINT ( 'NONE',  ( 219.5005434568853673, 10.59938867211075042, -9.448537646917804622 ) ) ;
#7676 = AXIS2_PLACEMENT_3D ( 'NONE', #14125, #14333, #9627 ) ;
#7677 = CARTESIAN_POINT ( 'NONE',  ( 219.1036532380573192, 37.34809784919840325, -17.20332536629370068 ) ) ;
#7678 = EDGE_CURVE ( 'NONE', #11054, #862, #7078, .T. ) ;
#7679 = CARTESIAN_POINT ( 'NONE',  ( 214.9776847560361830, 7.988114983668789471, -4.409371045253012156 ) ) ;
#7680 = EDGE_CURVE ( 'NONE', #13711, #17780, #5493, .T. ) ;
#7681 = ORIENTED_EDGE ( 'NONE', *, *, #15423, .F. ) ;
#7682 = DIRECTION ( 'NONE',  ( -0.4272097022732527227, 0.7399489098236350371, 0.5195839500354227924 ) ) ;
#7683 = EDGE_LOOP ( 'NONE', ( #20076, #1556, #10256, #19255 ) ) ;
#7684 = CARTESIAN_POINT ( 'NONE',  ( 220.6020034895022945, 34.75287908616212462, -10.17395310825082433 ) ) ;
#7685 = CARTESIAN_POINT ( 'NONE',  ( -31.74999999999995737, 0.000000000000000000, 0.000000000000000000 ) ) ;
#7686 = CARTESIAN_POINT ( 'NONE',  ( 200.4130575059754733, 6.471181724797008705, -24.79563718815128226 ) ) ;
#7687 = EDGE_CURVE ( 'NONE', #16560, #13544, #4220, .T. ) ;
#7688 = LINE ( 'NONE', #20417, #19174 ) ;
#7689 = AXIS2_PLACEMENT_3D ( 'NONE', #16852, #8896, #18552 ) ;
#7690 = CARTESIAN_POINT ( 'NONE',  ( 5.000000000000004441, 0.000000000000000000, 0.000000000000000000 ) ) ;
#7691 = ORIENTED_EDGE ( 'NONE', *, *, #9457, .T. ) ;
#7692 = VERTEX_POINT ( 'NONE', #15378 ) ;
#7693 = CIRCLE ( 'NONE', #1284, 12.47473710546057823 ) ;
#7694 = CYLINDRICAL_SURFACE ( 'NONE', #18942, 3.902363844300889451 ) ;
#7695 = EDGE_CURVE ( 'NONE', #16603, #15193, #13873, .T. ) ;
#7696 = CARTESIAN_POINT ( 'NONE',  ( 210.9359965013291003, 12.90064274403945532, -3.481206571632993629 ) ) ;
#7697 = CARTESIAN_POINT ( 'NONE',  ( -6.200167922753938576, 50.40944506478484044, -7.783125444142615201 ) ) ;
#7698 = DIRECTION ( 'NONE',  ( 0.8660254037844380415, 0.5000000000000008882, 0.000000000000000000 ) ) ;
#7699 = ADVANCED_FACE ( 'NONE', ( #15274 ), #5580, .T. ) ;
#7700 = CARTESIAN_POINT ( 'NONE',  ( 28.42607121268105175, 178.7209698509877285, 11.00000000000001243 ) ) ;
#7701 = CARTESIAN_POINT ( 'NONE',  ( 96.88087538439037871, 198.6134603144003563, 11.00000000000000888 ) ) ;
#7702 = VECTOR ( 'NONE', #3420, 1000.000000000000114 ) ;
#7704 = ORIENTED_EDGE ( 'NONE', *, *, #10765, .F. ) ;
#7703 = VERTEX_POINT ( 'NONE', #16939 ) ;
#7705 = ORIENTED_EDGE ( 'NONE', *, *, #16391, .F. ) ;
#7706 = CARTESIAN_POINT ( 'NONE',  ( 195.3764439868359943, 3.740314234153661488, -16.84511136304289991 ) ) ;
#7707 = PLANE ( 'NONE',  #19655 ) ;
#7708 = EDGE_CURVE ( 'NONE', #8493, #18834, #6135, .T. ) ;
#7709 = VECTOR ( 'NONE', #3915, 999.9999999999998863 ) ;
#7710 = CARTESIAN_POINT ( 'NONE',  ( -2.573654215855741612, 77.12664207850482967, -3.593879484356239828 ) ) ;
#7711 = EDGE_LOOP ( 'NONE', ( #9404, #4650, #3743, #1891 ) ) ;
#7712 = EDGE_LOOP ( 'NONE', ( #20486, #14300 ) ) ;
#7713 = LINE ( 'NONE', #9292, #5793 ) ;
#7714 = DIRECTION ( 'NONE',  ( 0.9463560092124702061, -0.3231258328073551289, 9.221751860358058811E-17 ) ) ;
#7715 = CARTESIAN_POINT ( 'NONE',  ( 1.402599256620770118, 52.27665093585768830, -4.545845583688177705 ) ) ;
#7716 = FACE_OUTER_BOUND ( 'NONE', #2254, .T. ) ;
#7717 = ORIENTED_EDGE ( 'NONE', *, *, #4508, .T. ) ;
#7718 = EDGE_CURVE ( 'NONE', #17213, #1051, #8288, .T. ) ;
#7719 = ADVANCED_FACE ( 'NONE', ( #10570 ), #10127, .T. ) ;
#7720 = EDGE_LOOP ( 'NONE', ( #18727, #12927, #2981, #10137 ) ) ;
#7721 = CARTESIAN_POINT ( 'NONE',  ( 1.484819526751601559, 76.25000000000000000, -2.578432583507792142 ) ) ;
#7722 = CARTESIAN_POINT ( 'NONE',  ( 193.8010743977839354, 17.92347240697177568, -24.79563718815128226 ) ) ;
#7723 = CIRCLE ( 'NONE', #8736, 0.4000000000000001887 ) ;
#7724 = CARTESIAN_POINT ( 'NONE',  ( 8.399999999999998579, 0.000000000000000000, 4.000000000000000000 ) ) ;
#7725 = CARTESIAN_POINT ( 'NONE',  ( 211.7854512130869580, 13.56808555472074751, -4.379064819896290928 ) ) ;
#7726 = ADVANCED_FACE ( 'NONE', ( #15065 ), #4424, .T. ) ;
#7727 = FACE_OUTER_BOUND ( 'NONE', #8386, .T. ) ;
#7728 = DIRECTION ( 'NONE',  ( 1.000000000000000000, 0.000000000000000000, 0.000000000000000000 ) ) ;
#7729 = CARTESIAN_POINT ( 'NONE',  ( -20.99191269157562090, 15.42836575585571879, 11.45997927866226185 ) ) ;
#7730 = CARTESIAN_POINT ( 'NONE',  ( -28.80487160773575184, 69.93605911897407168, 1.714708221108182551 ) ) ;
#7731 = CARTESIAN_POINT ( 'NONE',  ( 219.1067971192485686, 36.72480411789796051, -17.14987233279964229 ) ) ;
#7732 = DIRECTION ( 'NONE',  ( -1.000000000000000000, 0.000000000000000000, 0.000000000000000000 ) ) ;
#7733 = ORIENTED_EDGE ( 'NONE', *, *, #2828, .F. ) ;
#7734 = EDGE_CURVE ( 'NONE', #11978, #5258, #10775, .T. ) ;
#7735 = CARTESIAN_POINT ( 'NONE',  ( 82.29545726055718546, 62.24665149762746807, 0.2089934920557551534 ) ) ;
#7736 = B_SPLINE_CURVE_WITH_KNOTS ( 'NONE', 3,
 ( #10922, #7628, #16973, #20352 ),
 .UNSPECIFIED., .F., .F.,
 ( 4, 4 ),
 ( 4.203583919701888644E-07, 0.0008544060963714298707 ),
 .UNSPECIFIED. ) ;
#7737 = ORIENTED_EDGE ( 'NONE', *, *, #11594, .T. ) ;
#7738 = CIRCLE ( 'NONE', #16884, 3.902363844300875240 ) ;
#7739 = ORIENTED_EDGE ( 'NONE', *, *, #17717, .T. ) ;
#7740 = CARTESIAN_POINT ( 'NONE',  ( 0.6310778956523167560, 71.62317011047247206, 0.9609777548054254659 ) ) ;
#7741 = EDGE_CURVE ( 'NONE', #10069, #7744, #13554, .T. ) ;
#7742 = CONTEXT_DEPENDENT_SHAPE_REPRESENTATION ( #7169, #19887 ) ;
#7743 = LINE ( 'NONE', #16135, #17058 ) ;
#7744 = VERTEX_POINT ( 'NONE', #20740 ) ;
#7745 = LINE ( 'NONE', #7424, #19897 ) ;
#7746 = CYLINDRICAL_SURFACE ( 'NONE', #18918, 3.902363844300889451 ) ;
#7747 = DIRECTION ( 'NONE',  ( -0.5000000000000049960, 0.8660254037844357100, -0.000000000000000000 ) ) ;
#7748 = CARTESIAN_POINT ( 'NONE',  ( 34.99529059433362477, 263.3427481158986438, 1.000000000000017097 ) ) ;
#7749 = AXIS2_PLACEMENT_3D ( 'NONE', #13344, #9925, #16420 ) ;
#7750 = ORIENTED_EDGE ( 'NONE', *, *, #4432, .F. ) ;
#7751 = CARTESIAN_POINT ( 'NONE',  ( -46.99999999999998579, 64.25000000000000000, -2.528164662410438357 ) ) ;
#7752 = LINE ( 'NONE', #17100, #8540 ) ;
#7753 = CARTESIAN_POINT ( 'NONE',  ( 206.2654030616020293, 10.38108426852119415, -14.49413924534530551 ) ) ;
#7754 = CARTESIAN_POINT ( 'NONE',  ( 4.000000000000000000, 5.278424836066145431, -3.047500000000006093 ) ) ;
#7755 = DIRECTION ( 'NONE',  ( 1.000000000000000000, 0.000000000000000000, 0.000000000000000000 ) ) ;
#7756 = ORIENTED_EDGE ( 'NONE', *, *, #8614, .T. ) ;
#7757 = CARTESIAN_POINT ( 'NONE',  ( 212.1242269781990899, 6.340670367513290273, -26.58724934764018855 ) ) ;
#7758 = CARTESIAN_POINT ( 'NONE',  ( -4.115175346691388292, 73.88542888634934513, 3.878668165723258010 ) ) ;
#7759 = CYLINDRICAL_SURFACE ( 'NONE', #3368, 15.00000000000001954 ) ;
#7760 = CARTESIAN_POINT ( 'NONE',  ( -28.99999999999999289, 0.000000000000000000, 15.00000000000000178 ) ) ;
#7761 = FACE_OUTER_BOUND ( 'NONE', #11724, .T. ) ;
#7763 = VERTEX_POINT ( 'NONE', #7494 ) ;
#7762 = ORIENTED_EDGE ( 'NONE', *, *, #5363, .T. ) ;
#7764 = VECTOR ( 'NONE', #722, 1000.000000000000114 ) ;
#7765 = DIRECTION ( 'NONE',  ( -0.5000000000000047740, 0.8660254037844358210, 0.000000000000000000 ) ) ;
#7766 = SURFACE_STYLE_FILL_AREA ( #10962 ) ;
#7767 = VECTOR ( 'NONE', #6310, 1000.000000000000000 ) ;
#7768 = FACE_OUTER_BOUND ( 'NONE', #13859, .T. ) ;
#7769 = CARTESIAN_POINT ( 'NONE',  ( 201.0525450381139194, 0.7212519096665224172, -23.06309126349794525 ) ) ;
#7770 = CARTESIAN_POINT ( 'NONE',  ( 208.4761278624580711, 5.007259451653140125, -14.00000000000005507 ) ) ;
#7771 = VECTOR ( 'NONE', #16154, 1000.000000000000000 ) ;
#7772 = ORIENTED_EDGE ( 'NONE', *, *, #3256, .F. ) ;
#7773 = EDGE_CURVE ( 'NONE', #4169, #19778, #4633, .T. ) ;
#7774 = DIRECTION ( 'NONE',  ( -0.8660254037844360431, -0.5000000000000044409, 5.976026924694052093E-17 ) ) ;
#7775 = DIRECTION ( 'NONE',  ( 1.000000000000000000, 0.000000000000000000, 0.000000000000000000 ) ) ;
#7776 = ORIENTED_EDGE ( 'NONE', *, *, #18872, .T. ) ;
#7777 = CARTESIAN_POINT ( 'NONE',  ( 212.9190227734775078, 14.22255340025794190, -23.49337750257581803 ) ) ;
#7778 = LINE ( 'NONE', #3222, #16174 ) ;
#7779 = VECTOR ( 'NONE', #16686, 1000.000000000000114 ) ;
#7780 = CARTESIAN_POINT ( 'NONE',  ( -14.99999999999999645, 0.000000000000000000, 15.00000000000000000 ) ) ;
#7781 = CARTESIAN_POINT ( 'NONE',  ( 177.1791022559528983, 56.75747545832872731, -29.00000000000007105 ) ) ;
#7782 = ORIENTED_EDGE ( 'NONE', *, *, #11895, .T. ) ;
#7783 = CARTESIAN_POINT ( 'NONE',  ( 5.000000000000000000, 7.027796151710712813, -4.057500000000007212 ) ) ;
#7784 = EDGE_CURVE ( 'NONE', #15951, #4803, #11099, .T. ) ;
#7785 = ORIENTED_EDGE ( 'NONE', *, *, #14511, .T. ) ;
#7786 = ORIENTED_EDGE ( 'NONE', *, *, #17691, .F. ) ;
#7787 = FACE_OUTER_BOUND ( 'NONE', #2904, .T. ) ;
#7788 = CARTESIAN_POINT ( 'NONE',  ( -15.99999999999999289, 0.000000000000000000, 0.000000000000000000 ) ) ;
#7789 = CARTESIAN_POINT ( 'NONE',  ( 221.4896362261276863, 32.59760571852110189, -15.81459191843843648 ) ) ;
#7790 = AXIS2_PLACEMENT_3D ( 'NONE', #9122, #10501, #14144 ) ;
#7791 = DIRECTION ( 'NONE',  ( 0.5000000000000054401, -0.8660254037844354880, 0.000000000000000000 ) ) ;
#7792 = DIRECTION ( 'NONE',  ( 1.000000000000000000, -0.000000000000000000, -0.000000000000000000 ) ) ;
#7793 = CIRCLE ( 'NONE', #20657, 8.000000000000000000 ) ;
#7794 = EDGE_CURVE ( 'NONE', #2559, #13175, #6101, .T. ) ;
#7795 = ORIENTED_EDGE ( 'NONE', *, *, #12555, .F. ) ;
#7796 = EDGE_LOOP ( 'NONE', ( #8087, #4179, #4809, #5274 ) ) ;
#7797 = VECTOR ( 'NONE', #18909, 1000.000000000000000 ) ;
#7798 = EDGE_CURVE ( 'NONE', #1811, #15672, #4322, .T. ) ;
#7799 = DIRECTION ( 'NONE',  ( 0.8645602258681718277, 0.4991540791356397500, 0.05814482891046558743 ) ) ;
#7800 = VECTOR ( 'NONE', #11342, 1000.000000000000227 ) ;
#7801 = CARTESIAN_POINT ( 'NONE',  ( -3.775565802572502960, 47.04367182761800592, -2.628322306727621349 ) ) ;
#7802 = FACE_OUTER_BOUND ( 'NONE', #6805, .T. ) ;
#7803 = DIRECTION ( 'NONE',  ( 0.8660254037844361541, 0.5000000000000044409, -5.976026924694052093E-17 ) ) ;
#7804 = VECTOR ( 'NONE', #19785, 1000.000000000000227 ) ;
#7805 = LINE ( 'NONE', #14201, #5944 ) ;
#7807 = VERTEX_POINT ( 'NONE', #5997 ) ;
#7806 = ORIENTED_EDGE ( 'NONE', *, *, #6755, .T. ) ;
#7808 = AXIS2_PLACEMENT_3D ( 'NONE', #11006, #17578, #17259 ) ;
#7809 = CARTESIAN_POINT ( 'NONE',  ( 32.36389338619004263, 157.9004617752989930, 4.000000000000000000 ) ) ;
#7810 = CARTESIAN_POINT ( 'NONE',  ( 218.7128531318510625, 38.02498348875093370, -16.48323849494058635 ) ) ;
#7811 = CARTESIAN_POINT ( 'NONE',  ( 209.9156946368443357, 16.61257900951069288, -4.494676796018852727 ) ) ;
#7812 = VECTOR ( 'NONE', #10115, 1000.000000000000114 ) ;
#7813 = EDGE_LOOP ( 'NONE', ( #9275, #14784, #14965, #3182, #7415, #13670, #2218, #8373, #178, #7616, #2742, #17036, #11607, #10336, #1308, #10303, #13769, #2597, #8191, #6491, #18080, #3724, #9862, #14963, #2265, #12944, #10585, #20747, #9450, #8569, #12945, #15777, #11740, #3647, #3419, #9736, #20900, #6595, #6899, #2428, #17660, #18258, #12818, #19848, #17787, #2128, #13564, #14069, #9562, #1838, #7462, #13107, #19567, #5098, #7938, #4905, #4541, #18119, #17610, #13269, #19345, #20125, #7126, #16949, #17839, #6475, #6794, #10669, #14013, #6950, #4576, #16704, #3799, #20430, #18951, #12817, #12201, #5548, #15691, #1822, #7962, #14725, #3562, #7111, #5908, #14539, #1736, #712, #17502, #6203, #9982, #14017, #7871, #15184, #20332, #13654, #1133, #1004, #9264, #5540, #1059, #19976, #10379, #717, #8315, #11015, #17287, #6061 ) ) ;
#7814 = VERTEX_POINT ( 'NONE', #17366 ) ;
#7815 = ADVANCED_BREP_SHAPE_REPRESENTATION ( '', ( #3331, #18233 ), #14188 ) ;
#7816 = CARTESIAN_POINT ( 'NONE',  ( 216.7268875047958829, 8.998017661532479394, -6.310089745291985963 ) ) ;
#7817 = CARTESIAN_POINT ( 'NONE',  ( 172.0049095375684090, -3.964873019432338275, -29.00000000000001066 ) ) ;
#7818 = CARTESIAN_POINT ( 'NONE',  ( -19.14637054419212348, 50.42580415542552430, -16.04958827719470094 ) ) ;
#7819 = CARTESIAN_POINT ( 'NONE',  ( 202.6305150283801026, 8.282480684066333865, -25.48492467622465441 ) ) ;
#7820 = ORIENTED_EDGE ( 'NONE', *, *, #13114, .T. ) ;
#7821 = EDGE_CURVE ( 'NONE', #16283, #4229, #14305, .T. ) ;
#7822 = ORIENTED_EDGE ( 'NONE', *, *, #14106, .F. ) ;
#7823 = CARTESIAN_POINT ( 'NONE',  ( 0.9890147436984468854, 73.25359183295171306, 0.03495786392107397972 ) ) ;
#7824 = EDGE_CURVE ( 'NONE', #2011, #12209, #9125, .T. ) ;
#7825 = VECTOR ( 'NONE', #1140, 1000.000000000000227 ) ;
#7826 = CARTESIAN_POINT ( 'NONE',  ( 227.1552142281217925, 41.27103037639910355, -10.80501622924628258 ) ) ;
#7827 = VECTOR ( 'NONE', #7243, 1000.000000000000227 ) ;
#7828 = EDGE_CURVE ( 'NONE', #16338, #600, #2738, .T. ) ;
#7829 = CIRCLE ( 'NONE', #6810, 3.902363844300875240 ) ;
#7830 = CARTESIAN_POINT ( 'NONE',  ( 218.9076280839623223, 35.55626861788439896, -17.48830818005195908 ) ) ;
#7831 = CARTESIAN_POINT ( 'NONE',  ( -31.85409535283075044, 63.41252023259978898, 2.433313739304557188 ) ) ;
#7832 = CARTESIAN_POINT ( 'NONE',  ( 62.36299956745850892, 74.53177739387973588, -21.35531421961401222 ) ) ;
#7833 = CARTESIAN_POINT ( 'NONE',  ( 229.4623969809411506, 36.29540673510603455, -14.55761806292095706 ) ) ;
#7834 = DIRECTION ( 'NONE',  ( 0.1503837331804443733, 0.08682408883347179918, 0.9848077530122060219 ) ) ;
#7835 = DIRECTION ( 'NONE',  ( 0.5000000000000054401, -0.8660254037844354880, 0.000000000000000000 ) ) ;
#7836 = EDGE_CURVE ( 'NONE', #15363, #694, #19059, .T. ) ;
#7837 = ORIENTED_EDGE ( 'NONE', *, *, #2261, .T. ) ;
#7838 = CARTESIAN_POINT ( 'NONE',  ( 82.25636457018906356, 63.72284541912095079, 0.4406977701249564228 ) ) ;
#7839=STYLED_ITEM('',(#20995),#3258);
#7840 = VERTEX_POINT ( 'NONE', #7905 ) ;
#7841 = CARTESIAN_POINT ( 'NONE',  ( -4.425686930326540924, 71.02946758568734253, 4.727326826883592403 ) ) ;
#7842 = VECTOR ( 'NONE', #11783, 1000.000000000000000 ) ;
#7843 = CARTESIAN_POINT ( 'NONE',  ( 5.000000000000004441, 0.000000000000000000, 0.000000000000000000 ) ) ;
#7844 = AXIS2_PLACEMENT_3D ( 'NONE', #18690, #18583, #13924 ) ;
#7845 = EDGE_CURVE ( 'NONE', #15359, #3226, #15883, .T. ) ;
#7846 = AXIS2_PLACEMENT_3D ( 'NONE', #4493, #12451, #14155 ) ;
#7847 = DIRECTION ( 'NONE',  ( 0.8660254037844360431, 0.5000000000000044409, -5.976026924694053325E-17 ) ) ;
#7848 = APPLICATION_PROTOCOL_DEFINITION ( 'draft international standard', 'automotive_design', 1998, #13525 ) ;
#7849 = EDGE_CURVE ( 'NONE', #8938, #20059, #15995, .T. ) ;
#7850 = DIRECTION ( 'NONE',  ( -0.5000000000000045519, 0.8660254037844361541, 0.000000000000000000 ) ) ;
#7851 = ORIENTED_EDGE ( 'NONE', *, *, #20901, .F. ) ;
#7852 = DIRECTION ( 'NONE',  ( 0.000000000000000000, 0.000000000000000000, -1.000000000000000000 ) ) ;
#7853 = ADVANCED_FACE ( 'NONE', ( #1355 ), #17152, .F. ) ;
#7854 = DIRECTION ( 'NONE',  ( -0.8660254037844361541, -0.5000000000000042188, 6.872020471724001723E-17 ) ) ;
#7855 = CARTESIAN_POINT ( 'NONE',  ( 211.0966947254765103, 27.85633560694163791, -15.52474636582213563 ) ) ;
#7856 = CARTESIAN_POINT ( 'NONE',  ( 208.5367637565365726, 11.69245497716839566, -11.22024895763578556 ) ) ;
#7857 = ORIENTED_EDGE ( 'NONE', *, *, #14172, .T. ) ;
#7858 = DIRECTION ( 'NONE',  ( 0.5000000000000054401, -0.8660254037844354880, 0.000000000000000000 ) ) ;
#7859 = CARTESIAN_POINT ( 'NONE',  ( 210.7763206480203166, 12.98546375133203767, -24.38552490958320718 ) ) ;
#7860 = EDGE_CURVE ( 'NONE', #3143, #20843, #12150, .T. ) ;
#7861 = AXIS2_PLACEMENT_3D ( 'NONE', #12066, #2419, #4111 ) ;
#7862 = DIRECTION ( 'NONE',  ( -0.8660254037844355990, -0.5000000000000054401, 8.343535232742331521E-16 ) ) ;
#7863 = DIRECTION ( 'NONE',  ( 0.8660254037844375974, 0.5000000000000019984, -2.775557561562891844E-16 ) ) ;
#7864 = FACE_OUTER_BOUND ( 'NONE', #4262, .T. ) ;
#7865 = ORIENTED_EDGE ( 'NONE', *, *, #589, .F. ) ;
#7866 = DIRECTION ( 'NONE',  ( -0.8660254037844360431, -0.5000000000000045519, 5.976026924694054558E-17 ) ) ;
#7867 = CARTESIAN_POINT ( 'NONE',  ( 59.65508358009556389, 84.67062659264655622, -8.767208989671093633 ) ) ;
#7868 = CARTESIAN_POINT ( 'NONE',  ( 45.00000000000000000, 5.000000000000000000, 15.00000000000000000 ) ) ;
#7869 = CARTESIAN_POINT ( 'NONE',  ( -33.20451348466885833, 77.44204738084620487, -4.113378397039106460 ) ) ;
#7870 = EDGE_CURVE ( 'NONE', #5809, #9014, #1020, .T. ) ;
#7872 = ORIENTED_EDGE ( 'NONE', *, *, #15618, .T. ) ;
#7871 = ORIENTED_EDGE ( 'NONE', *, *, #8069, .F. ) ;
#7873 = ORIENTED_EDGE ( 'NONE', *, *, #14321, .T. ) ;
#7874 = CONICAL_SURFACE ( 'NONE', #8558, 4.509097725792825528, 0.5235987755983015912 ) ;
#7875 = CARTESIAN_POINT ( 'NONE',  ( 215.5731683782092034, 15.75492507961826227, -16.70797078425240301 ) ) ;
#7876 = ORIENTED_EDGE ( 'NONE', *, *, #8104, .F. ) ;
#7877 = EDGE_CURVE ( 'NONE', #4705, #11414, #11001, .T. ) ;
#7878 = CARTESIAN_POINT ( 'NONE',  ( -29.22340388804807532, 78.20541348178687713, -5.222231676846088355 ) ) ;
#7879 = CARTESIAN_POINT ( 'NONE',  ( 198.7478178127443016, -1.382203064952688409, -11.23040475586387821 ) ) ;
#7880 = CARTESIAN_POINT ( 'NONE',  ( -11.68625644715183931, 65.74999999999995737, -2.528164662410434804 ) ) ;
#7881 = ORIENTED_EDGE ( 'NONE', *, *, #13, .F. ) ;
#7882 = CARTESIAN_POINT ( 'NONE',  ( 210.6201421056092897, 5.472286561439484665, -25.76107385416583639 ) ) ;
#7883 = PLANE ( 'NONE',  #4316 ) ;
#7884 = CIRCLE ( 'NONE', #457, 11.98469917212512215 ) ;
#7885 = DIRECTION ( 'NONE',  ( 0.4999999999999995004, -0.8660254037844390407, 0.000000000000000000 ) ) ;
#7886 = DIRECTION ( 'NONE',  ( 0.000000000000000000, 0.000000000000000000, -1.000000000000000000 ) ) ;
#7887 = ORIENTED_EDGE ( 'NONE', *, *, #8024, .F. ) ;
#7888 = DIRECTION ( 'NONE',  ( 0.5000000000000045519, -0.8660254037844360431, 0.000000000000000000 ) ) ;
#7889 = ORIENTED_EDGE ( 'NONE', *, *, #15805, .F. ) ;
#7890 = ORIENTED_EDGE ( 'NONE', *, *, #6118, .F. ) ;
#7891 = EDGE_CURVE ( 'NONE', #10811, #14523, #20527, .T. ) ;
#7892 = CARTESIAN_POINT ( 'NONE',  ( 200.8776667170992027, -0.1525342266901607846, -21.66653917424381603 ) ) ;
#7893 = PLANE ( 'NONE',  #4109 ) ;
#7894 = CARTESIAN_POINT ( 'NONE',  ( 207.4990653133776277, 25.83201114944695220, -5.993340328401894901 ) ) ;
#7895 = LINE ( 'NONE', #14397, #5604 ) ;
#7896 = CARTESIAN_POINT ( 'NONE',  ( 200.6602785227575225, -0.02044413540491671344, -6.204501730076046329 ) ) ;
#7897 = VECTOR ( 'NONE', #17724, 999.9999999999998863 ) ;
#7898 = VECTOR ( 'NONE', #12858, 1000.000000000000227 ) ;
#7899 = VERTEX_POINT ( 'NONE', #20939 ) ;
#7900 = CARTESIAN_POINT ( 'NONE',  ( 197.5856452450873917, 5.015797175299181454, -21.91826003371427944 ) ) ;
#7901 = DIRECTION ( 'NONE',  ( -0.5000000000000045519, 0.8660254037844360431, 0.000000000000000000 ) ) ;
#7902 = EDGE_CURVE ( 'NONE', #20338, #1345, #4402, .T. ) ;
#7903 = CARTESIAN_POINT ( 'NONE',  ( -6.518053481867566390, 50.25229571315650645, -8.166628857475616954 ) ) ;
#7904 = CARTESIAN_POINT ( 'NONE',  ( 215.1183575532813848, 35.36044452787341186, -14.00000000000004441 ) ) ;
#7905 = CARTESIAN_POINT ( 'NONE',  ( -15.99999999999999289, 9.999999999999994671, -12.50000000000000000 ) ) ;
#7906 = CARTESIAN_POINT ( 'NONE',  ( 218.2848876630777397, 36.63488666678333061, -16.94731950718122704 ) ) ;
#7908 = VERTEX_POINT ( 'NONE', #17775 ) ;
#7907 = EDGE_LOOP ( 'NONE', ( #2391, #9683, #1315, #18520, #17641, #13929 ) ) ;
#7909 = VERTEX_POINT ( 'NONE', #10003 ) ;
#7910 = CARTESIAN_POINT ( 'NONE',  ( -35.00000000000000000, 65.00000000000000000, -12.50000000000000000 ) ) ;
#7911 = DIRECTION ( 'NONE',  ( 0.5000000000000052180, -0.8660254037844355990, -1.665334536937734318E-16 ) ) ;
#7912 = CARTESIAN_POINT ( 'NONE',  ( -4.591091843082831581, 79.34446119966882804, -7.911977669603137642 ) ) ;
#7913 = ORIENTED_EDGE ( 'NONE', *, *, #10333, .F. ) ;
#7914 = ORIENTED_EDGE ( 'NONE', *, *, #20504, .F. ) ;
#7915 = EDGE_LOOP ( 'NONE', ( #834, #17418, #937, #20601 ) ) ;
#7916 = EDGE_CURVE ( 'NONE', #13099, #7029, #9805, .T. ) ;
#7917 = DIRECTION ( 'NONE',  ( 0.5330816498126389469, -0.8460638005688666530, 0.000000000000000000 ) ) ;
#7918 = DIRECTION ( 'NONE',  ( 0.9736467517689000317, -0.2280614013152375275, 0.000000000000000000 ) ) ;
#7919 = CARTESIAN_POINT ( 'NONE',  ( -32.95070415583882806, 56.92051799503307308, 0.1616960027641645703 ) ) ;
#7920 = CARTESIAN_POINT ( 'NONE',  ( -28.22159099458506404, 8.920131004072807457, -2.707279339256349004 ) ) ;
#7921 = EDGE_LOOP ( 'NONE', ( #4815, #10742, #9481, #6390 ) ) ;
#7922 = EDGE_LOOP ( 'NONE', ( #11863, #6111, #10020, #18675 ) ) ;
#7923 = LINE ( 'NONE', #20546, #9711 ) ;
#7924 = AXIS2_PLACEMENT_3D ( 'NONE', #5862, #12359, #18815 ) ;
#7925 = CARTESIAN_POINT ( 'NONE',  ( 9.999999999999998224, 0.000000000000000000, -5.400000000000001243 ) ) ;
#7926 = EDGE_CURVE ( 'NONE', #13130, #14216, #9699, .T. ) ;
#7927 = CARTESIAN_POINT ( 'NONE',  ( 199.6438684810882762, -0.8648679703767148119, -19.29168348739290906 ) ) ;
#7928 = CARTESIAN_POINT ( 'NONE',  ( -27.49344780102824259, 60.03966354978251019, 4.915051137978660556 ) ) ;
#7929 = DIRECTION ( 'NONE',  ( 0.5000000000000007772, -0.8660254037844381525, 0.000000000000000000 ) ) ;
#7930 = ORIENTED_EDGE ( 'NONE', *, *, #20095, .T. ) ;
#7931 = CARTESIAN_POINT ( 'NONE',  ( -14.99999999999999645, -9.999999999999998224, -15.00000000000000000 ) ) ;
#7932 = CARTESIAN_POINT ( 'NONE',  ( 203.6701878702990598, 1.459728612827534855, -3.762296834228767928 ) ) ;
#7933 = CARTESIAN_POINT ( 'NONE',  ( 195.6699422177752581, 3.732742836357164862, -18.25196083293855054 ) ) ;
#7934 = ORIENTED_EDGE ( 'NONE', *, *, #3688, .F. ) ;
#7935 = B_SPLINE_CURVE_WITH_KNOTS ( 'NONE', 3,
 ( #20442, #7506, #14215, #10680 ),
 .UNSPECIFIED., .F., .F.,
 ( 4, 4 ),
 ( 8.673617379884035472E-19, 0.001416029653784999084 ),
 .UNSPECIFIED. ) ;
#7936 = CARTESIAN_POINT ( 'NONE',  ( 81.27003798075334373, 65.71846927405951533, 0.4875263538762131255 ) ) ;
#7937 = EDGE_CURVE ( 'NONE', #2596, #38, #20300, .T. ) ;
#7938 = ORIENTED_EDGE ( 'NONE', *, *, #20264, .F. ) ;
#7939 = EDGE_CURVE ( 'NONE', #19075, #3563, #15919, .T. ) ;
#7940 = ORIENTED_EDGE ( 'NONE', *, *, #15347, .T. ) ;
#7941 = CARTESIAN_POINT ( 'NONE',  ( -2.659465448949789756, 64.25000000000001421, 3.134647201270585271 ) ) ;
#7942 = FACE_OUTER_BOUND ( 'NONE', #13543, .T. ) ;
#7943 = TOROIDAL_SURFACE ( 'NONE', #17148, 5.400000000000000355, 0.4000000000000000222 ) ;
#7944 = CARTESIAN_POINT ( 'NONE',  ( 221.8183460879464803, 32.23418173770701856, -14.95362368770818051 ) ) ;
#7945 = EDGE_LOOP ( 'NONE', ( #6951, #637, #19787, #11696 ) ) ;
#7946 = CONTEXT_DEPENDENT_SHAPE_REPRESENTATION ( #17866, #956 ) ;
#7947 = CARTESIAN_POINT ( 'NONE',  ( 5.000000000000000000, 0.000000000000000000, 4.057500000000000107 ) ) ;
#7948 = ADVANCED_FACE ( 'NONE', ( #1976 ), #1349, .F. ) ;
#7949 = ORIENTED_EDGE ( 'NONE', *, *, #12208, .F. ) ;
#7950 = DIRECTION ( 'NONE',  ( 0.000000000000000000, 1.294035738186425244E-16, 1.000000000000000000 ) ) ;
#7951 = CARTESIAN_POINT ( 'NONE',  ( 206.6806582365933878, 10.62083195558484405, -12.63579004172483877 ) ) ;
#7952 = CARTESIAN_POINT ( 'NONE',  ( 209.1089911673190329, 31.29899458968461090, -15.52540737777744440 ) ) ;
#7953 = CARTESIAN_POINT ( 'NONE',  ( 184.9952905943349606, 3.535126980567727450, -29.00000000000001066 ) ) ;
#7954 = CARTESIAN_POINT ( 'NONE',  ( 195.0230325291159090, 3.359249353468287680, -14.01558723443171850 ) ) ;
#7955 = LINE ( 'NONE', #6458, #10564 ) ;
#7956 = VECTOR ( 'NONE', #13655, 1000.000000000000000 ) ;
#7957 = ADVANCED_FACE ( 'NONE', ( #11513 ), #11310, .F. ) ;
#7958 = CARTESIAN_POINT ( 'NONE',  ( 228.5305256799928486, 38.88892106552724215, -17.38313153181864124 ) ) ;
#7959 = FACE_OUTER_BOUND ( 'NONE', #12809, .T. ) ;
#7960 = DIRECTION ( 'NONE',  ( 0.4988343845952720179, -0.8640064986813590364, 0.06824241336467465335 ) ) ;
#7961 = AXIS2_PLACEMENT_3D ( 'NONE', #6986, #16544, #5080 ) ;
#7962 = ORIENTED_EDGE ( 'NONE', *, *, #3134, .F. ) ;
#7963 = AXIS2_PLACEMENT_3D ( 'NONE', #18239, #15300, #19924 ) ;
#7964 = DIRECTION ( 'NONE',  ( 0.5000000000000051070, -0.8660254037844359321, 0.000000000000000000 ) ) ;
#7965 = EDGE_CURVE ( 'NONE', #3973, #12454, #19667, .T. ) ;
#7966 = CARTESIAN_POINT ( 'NONE',  ( 80.73554840084692330, 67.38772768083256892, 0.5743335871849057916 ) ) ;
#7967 = CARTESIAN_POINT ( 'NONE',  ( 10.40000000000000036, 0.000000000000000000, 0.000000000000000000 ) ) ;
#7968 = CARTESIAN_POINT ( 'NONE',  ( -20.90620796478638610, 15.76932605263708886, 0.9645878285891481552 ) ) ;
#7970 = ORIENTED_EDGE ( 'NONE', *, *, #2675, .T. ) ;
#7969 = VERTEX_POINT ( 'NONE', #13327 ) ;
#7971 = ORIENTED_EDGE ( 'NONE', *, *, #3416, .T. ) ;
#7972 = AXIS2_PLACEMENT_3D ( 'NONE', #9585, #19353, #9892 ) ;
#7973 = VERTEX_POINT ( 'NONE', #83 ) ;
#7974 = EDGE_CURVE ( 'NONE', #470, #8218, #3458, .T. ) ;
#7975 = DIRECTION ( 'NONE',  ( 0.8660254037844352659, 0.5000000000000056621, 0.000000000000000000 ) ) ;
#7976 = EDGE_CURVE ( 'NONE', #6967, #4359, #9123, .T. ) ;
#7977 = ORIENTED_EDGE ( 'NONE', *, *, #13910, .F. ) ;
#7978 = VECTOR ( 'NONE', #15490, 1000.000000000000114 ) ;
#7979 = CARTESIAN_POINT ( 'NONE',  ( 228.1017308963825201, 39.63161541676044664, -10.39224118001587982 ) ) ;
#7980 = CIRCLE ( 'NONE', #6293, 12.47473710546057823 ) ;
#7981 = DIRECTION ( 'NONE',  ( 0.5000000000000043299, -0.8660254037844361541, -1.214306433183764966E-16 ) ) ;
#7982 = DIRECTION ( 'NONE',  ( 0.000000000000000000, -1.232415585510385534E-15, -1.000000000000000000 ) ) ;
#7983 = EDGE_CURVE ( 'NONE', #6933, #14685, #18274, .T. ) ;
#7984 = DIRECTION ( 'NONE',  ( -0.5000000000000051070, 0.8660254037844359321, -0.000000000000000000 ) ) ;
#7985 = DIRECTION ( 'NONE',  ( -1.000000000000000000, -0.000000000000000000, -0.000000000000000000 ) ) ;
#7986 = ORIENTED_EDGE ( 'NONE', *, *, #1246, .T. ) ;
#7987 = DIRECTION ( 'NONE',  ( 0.000000000000000000, 1.000000000000000000, -1.302777330458572662E-15 ) ) ;
#7988 = LINE ( 'NONE', #3333, #1383 ) ;
#7989 = AXIS2_PLACEMENT_3D ( 'NONE', #12163, #512, #16724 ) ;
#7990 = AXIS2_PLACEMENT_3D ( 'NONE', #17030, #3873, #701 ) ;
#7991 = DIRECTION ( 'NONE',  ( -0.5000000000000051070, 0.8660254037844359321, -0.000000000000000000 ) ) ;
#7992 = EDGE_CURVE ( 'NONE', #19959, #844, #14512, .T. ) ;
#7993 = VERTEX_POINT ( 'NONE', #19363 ) ;
#7994 = CARTESIAN_POINT ( 'NONE',  ( 208.8107687779841228, 4.427644383670616079, -14.00000000000005507 ) ) ;
#7995 = CARTESIAN_POINT ( 'NONE',  ( 199.2657312721003393, 25.05322593869168202, -14.00000000000005507 ) ) ;
#7996 = DIRECTION ( 'NONE',  ( -1.000000000000000000, -0.000000000000000000, -0.000000000000000000 ) ) ;
#7997 = DIRECTION ( 'NONE',  ( 1.000000000000000000, -0.000000000000000000, -0.000000000000000000 ) ) ;
#7998 = CARTESIAN_POINT ( 'NONE',  ( -25.99999999999999645, 9.999999999999994671, -7.499999999999998224 ) ) ;
#7999 = ORIENTED_EDGE ( 'NONE', *, *, #8178, .F. ) ;
#8000 = CIRCLE ( 'NONE', #2955, 5.000000000000001776 ) ;
#8001 = DIRECTION ( 'NONE',  ( 0.000000000000000000, 0.000000000000000000, -1.000000000000000000 ) ) ;
#8002 = LINE ( 'NONE', #16090, #12633 ) ;
#8003 = CARTESIAN_POINT ( 'NONE',  ( -12.36055546714704612, 49.51133710352112871, -11.98200832479694000 ) ) ;
#8004 = DIRECTION ( 'NONE',  ( 0.4953429730181640456, -0.8579591964396815484, 0.1361666490962538945 ) ) ;
#8005 = DIRECTION ( 'NONE',  ( 0.8660254037844360431, 0.5000000000000045519, 0.000000000000000000 ) ) ;
#8006 = DIRECTION ( 'NONE',  ( 0.000000000000000000, 0.000000000000000000, 1.000000000000000000 ) ) ;
#8007 = ORIENTED_EDGE ( 'NONE', *, *, #17949, .F. ) ;
#8008 = VERTEX_POINT ( 'NONE', #8322 ) ;
#8009 = CARTESIAN_POINT ( 'NONE',  ( -34.00000000000000711, 65.00000000000000000, -27.49999999999999645 ) ) ;
#8010 = CARTESIAN_POINT ( 'NONE',  ( -35.00000000000000000, 65.00000000000000000, -12.50000000000000000 ) ) ;
#8011 = CARTESIAN_POINT ( 'NONE',  ( 0.6071296115912496738, 78.11617769706943193, -5.220046598459772369 ) ) ;
#8012 = ORIENTED_EDGE ( 'NONE', *, *, #17437, .T. ) ;
#8013 = ORIENTED_EDGE ( 'NONE', *, *, #11585, .F. ) ;
#8014 = AXIS2_PLACEMENT_3D ( 'NONE', #12083, #18339, #7197 ) ;
#8015 = CARTESIAN_POINT ( 'NONE',  ( 226.6453546267926527, 41.17466721956452602, -10.52303454827235996 ) ) ;
#8016 = LINE ( 'NONE', #7058, #8477 ) ;
#8017 = CARTESIAN_POINT ( 'NONE',  ( 216.0745536026543334, 15.96406172101338683, -13.99136402100517174 ) ) ;
#8018 = DIRECTION ( 'NONE',  ( -1.060575238724903217E-16, -6.123233995736827666E-17, 1.000000000000000000 ) ) ;
#8019 = ORIENTED_EDGE ( 'NONE', *, *, #475, .T. ) ;
#8020 = ORIENTED_EDGE ( 'NONE', *, *, #2587, .F. ) ;
#8021 = CARTESIAN_POINT ( 'NONE',  ( 199.6091165883520659, 23.51942873589650773, -14.00000000000005507 ) ) ;
#8022 = PLANE ( 'NONE',  #20611 ) ;
#8023 = CIRCLE ( 'NONE', #17878, 5.999999999999998224 ) ;
#8024 = EDGE_CURVE ( 'NONE', #16809, #17637, #14825, .T. ) ;
#8025 = CARTESIAN_POINT ( 'NONE',  ( 211.0559258593130210, 13.14689389533870312, -25.15632882797110526 ) ) ;
#8026 = CARTESIAN_POINT ( 'NONE',  ( -28.92176035443840121, 57.78353514853240824, 0.6664698202380902048 ) ) ;
#8027 = DIRECTION ( 'NONE',  ( -0.000000000000000000, 1.000000000000000000, -0.000000000000000000 ) ) ;
#8028 = ORIENTED_EDGE ( 'NONE', *, *, #14866, .F. ) ;
#8029 = VECTOR ( 'NONE', #18510, 1000.000000000000227 ) ;
#8030 = FACE_OUTER_BOUND ( 'NONE', #9844, .T. ) ;
#8031 = CARTESIAN_POINT ( 'NONE',  ( 198.6293134455681013, -1.450621593242038099, -12.64773574313024440 ) ) ;
#8032 = ORIENTED_EDGE ( 'NONE', *, *, #17908, .T. ) ;
#8033 = B_SPLINE_CURVE_WITH_KNOTS ( 'NONE', 3,
 ( #4653, #20651, #11121, #11021 ),
 .UNSPECIFIED., .F., .F.,
 ( 4, 4 ),
 ( 2.239305297879237418E-05, 0.0005883192752736708447 ),
 .UNSPECIFIED. ) ;
#8034 = CARTESIAN_POINT ( 'NONE',  ( 62.76000446352012574, 78.08535740683855408, -12.62392526639253632 ) ) ;
#8035 = ORIENTED_EDGE ( 'NONE', *, *, #19283, .F. ) ;
#8036 = VERTEX_POINT ( 'NONE', #4838 ) ;
#8037 = CARTESIAN_POINT ( 'NONE',  ( 199.0943133668587564, -1.182153763511707867, -18.09983247376283089 ) ) ;
#8038 = CARTESIAN_POINT ( 'NONE',  ( 82.49529059433407951, 181.0703347563770365, 11.00000000000001066 ) ) ;
#8039 = ADVANCED_FACE ( 'NONE', ( #3245, #16495 ), #6516, .T. ) ;
#8040 = PRESENTATION_LAYER_ASSIGNMENT (  '', '', ( #5327 ) ) ;
#8041 = ORIENTED_EDGE ( 'NONE', *, *, #1901, .F. ) ;
#8042 = CARTESIAN_POINT ( 'NONE',  ( 226.6211368133091923, 39.11482588413117867, -14.00000000000005507 ) ) ;
#8043 = ORIENTED_EDGE ( 'NONE', *, *, #5529, .F. ) ;
#8044 = AXIS2_PLACEMENT_3D ( 'NONE', #7652, #14363, #10948 ) ;
#8045 = CARTESIAN_POINT ( 'NONE',  ( 5.000000000000004441, 2.342598717236899830, -4.057500000000030305 ) ) ;
#8046 = ORIENTED_EDGE ( 'NONE', *, *, #17646, .F. ) ;
#8047 = CARTESIAN_POINT ( 'NONE',  ( 208.8107687779841228, 4.427644383670616079, -14.00000000000005507 ) ) ;
#8048 = CARTESIAN_POINT ( 'NONE',  ( 208.9482664394169547, 31.70519001067595610, -14.65023073592818648 ) ) ;
#8049 = FACE_OUTER_BOUND ( 'NONE', #559, .T. ) ;
#8050 = EDGE_CURVE ( 'NONE', #13300, #15277, #17889, .T. ) ;
#8051 = EDGE_CURVE ( 'NONE', #10792, #18356, #390, .T. ) ;
#8052 = DIRECTION ( 'NONE',  ( 0.8660254037844362651, 0.5000000000000043299, 0.000000000000000000 ) ) ;
#8053 = LINE ( 'NONE', #11263, #9884 ) ;
#8054 = LINE ( 'NONE', #14562, #363 ) ;
#8055 = DIRECTION ( 'NONE',  ( 0.8660254037844370423, 0.5000000000000026645, -0.000000000000000000 ) ) ;
#8056 = CARTESIAN_POINT ( 'NONE',  ( 199.2542003381766449, 10.45716240621115745, -1.942038651984764330 ) ) ;
#8057 = VECTOR ( 'NONE', #7644, 1000.000000000000227 ) ;
#8058 = ORIENTED_EDGE ( 'NONE', *, *, #8050, .F. ) ;
#8059 = DIRECTION ( 'NONE',  ( -0.8660254037844354880, -0.5000000000000055511, 0.000000000000000000 ) ) ;
#8060 = CARTESIAN_POINT ( 'NONE',  ( 0.000000000000000000, -10.00000000000000000, 30.00000000000000000 ) ) ;
#8061 = EDGE_CURVE ( 'NONE', #6334, #791, #11207, .T. ) ;
#8062 = FACE_OUTER_BOUND ( 'NONE', #16745, .T. ) ;
#8063 = CARTESIAN_POINT ( 'NONE',  ( -28.80276981525291546, 76.40330993045616026, -2.758159894511351684 ) ) ;
#8065 = EDGE_LOOP ( 'NONE', ( #15250, #396, #15260, #13491, #13467, #7134, #7413 ) ) ;
#8064 = ORIENTED_EDGE ( 'NONE', *, *, #14113, .F. ) ;
#8066 = DIRECTION ( 'NONE',  ( -0.000000000000000000, -0.000000000000000000, 1.000000000000000000 ) ) ;
#8067 = UNCERTAINTY_MEASURE_WITH_UNIT (LENGTH_MEASURE( 1.000000000000000082E-05 ), #11108, 'distance_accuracy_value', 'NONE');
#8068 = ORIENTED_EDGE ( 'NONE', *, *, #14753, .F. ) ;
#8069 = EDGE_CURVE ( 'NONE', #9213, #19498, #10825, .T. ) ;
#8070 = CARTESIAN_POINT ( 'NONE',  ( 205.8264633344831225, 9.596613037118636669, -14.00000000000005507 ) ) ;
#8071 = AXIS2_PLACEMENT_3D ( 'NONE', #9944, #8367, #7095 ) ;
#8072 = VERTEX_POINT ( 'NONE', #10110 ) ;
#8073 = DIRECTION ( 'NONE',  ( 0.3200921998322429629, -0.5544159532159284032, -0.7682212795973754060 ) ) ;
#8074 = CARTESIAN_POINT ( 'NONE',  ( -29.10076314032669842, 78.36047030499236143, -5.510874449650665419 ) ) ;
#8075 = DIRECTION ( 'NONE',  ( 0.000000000000000000, -1.224646799147353207E-16, 1.000000000000000000 ) ) ;
#8076 = EDGE_CURVE ( 'NONE', #19534, #1937, #10467, .T. ) ;
#8077 = DIRECTION ( 'NONE',  ( 0.8660254037844357100, 0.5000000000000049960, -3.055037149610301786E-16 ) ) ;
#8078 = CARTESIAN_POINT ( 'NONE',  ( 72.75533871425699317, 69.93577090895743709, -0.4654751680537443925 ) ) ;
#8079 = DIRECTION ( 'NONE',  ( 0.8660254037844360431, 0.5000000000000044409, -5.976026924694053325E-17 ) ) ;
#8080 = VERTEX_POINT ( 'NONE', #11732 ) ;
#8081 = FACE_OUTER_BOUND ( 'NONE', #88, .T. ) ;
#8082 = CARTESIAN_POINT ( 'NONE',  ( 203.8492256719332829, 8.809093698002534722, -2.035916199211759370 ) ) ;
#8083 = EDGE_CURVE ( 'NONE', #5345, #12788, #13849, .T. ) ;
#8084 = VECTOR ( 'NONE', #11305, 999.9999999999998863 ) ;
#8085 = VERTEX_POINT ( 'NONE', #13533 ) ;
#8086 = CARTESIAN_POINT ( 'NONE',  ( 202.0125913935839037, 12.04972022458082037, -25.65046807331631129 ) ) ;
#8087 = ORIENTED_EDGE ( 'NONE', *, *, #13951, .F. ) ;
#8088 = CARTESIAN_POINT ( 'NONE',  ( 208.9425382666943847, 31.71895361803450086, -13.34399656285678581 ) ) ;
#8089 = DIRECTION ( 'NONE',  ( 0.000000000000000000, -1.000000000000000000, 0.000000000000000000 ) ) ;
#8090 = CARTESIAN_POINT ( 'NONE',  ( -31.74999999999995737, 0.000000000000000000, 0.000000000000000000 ) ) ;
#8091 = EDGE_CURVE ( 'NONE', #10891, #11555, #13948, .T. ) ;
#8092 = DIRECTION ( 'NONE',  ( 0.5000000000000054401, -0.8660254037844354880, 0.000000000000000000 ) ) ;
#8093 = CARTESIAN_POINT ( 'NONE',  ( -29.99999999999999645, 5.000000000000000888, -10.49999999999999822 ) ) ;
#8094 = CARTESIAN_POINT ( 'NONE',  ( 226.0093550869354715, 42.27625073618769846, -11.55788255683058807 ) ) ;
#8095 = EDGE_LOOP ( 'NONE', ( #15481, #15174, #19355, #11868 ) ) ;
#8096 = CARTESIAN_POINT ( 'NONE',  ( 77.47201823384298791, 70.53308754211151665, -25.18754646355691307 ) ) ;
#8097 = CARTESIAN_POINT ( 'NONE',  ( 201.5598379337182848, 7.133275713455735634, -25.46066938576250394 ) ) ;
#8098 = ADVANCED_FACE ( 'NONE', ( #19875 ), #13642, .T. ) ;
#8099 = AXIS2_PLACEMENT_3D ( 'NONE', #13113, #13014, #11411 ) ;
#8100 = ORIENTED_EDGE ( 'NONE', *, *, #5009, .F. ) ;
#8101 = CARTESIAN_POINT ( 'NONE',  ( 182.5734976231970563, 59.87193107572243633, -14.00000000000002842 ) ) ;
#8102 = CARTESIAN_POINT ( 'NONE',  ( -11.35743612562215787, 49.52957768806496119, -11.61502336121733769 ) ) ;
#8103 = CARTESIAN_POINT ( 'NONE',  ( 229.0669782285056328, 37.63328891968730971, -11.25902728360939697 ) ) ;
#8104 = EDGE_CURVE ( 'NONE', #4228, #3143, #2030, .T. ) ;
#8105 = DIRECTION ( 'NONE',  ( -0.5000000000000008882, 0.8660254037844381525, 0.000000000000000000 ) ) ;
#8106 = CARTESIAN_POINT ( 'NONE',  ( 79.36047190431935405, 49.50000000000002842, -12.49999999998710898 ) ) ;
#8107 = PRODUCT_DEFINITION ( 'UNKNOWN', '', #14550, #12563 ) ;
#8109 = ORIENTED_EDGE ( 'NONE', *, *, #19233, .F. ) ;
#8108 = EDGE_LOOP ( 'NONE', ( #13567, #15636, #18055, #12273 ) ) ;
#8110 = ORIENTED_EDGE ( 'NONE', *, *, #9143, .T. ) ;
#8111 = CARTESIAN_POINT ( 'NONE',  ( 45.89721438298043665, 238.4600622137188282, -13.99999999999998046 ) ) ;
#8112 = DIRECTION ( 'NONE',  ( -0.5000000000000051070, 0.8660254037844359321, -0.000000000000000000 ) ) ;
#8113 = CARTESIAN_POINT ( 'NONE',  ( -3.576301558931711533, 79.61691370731651318, -9.098688494705450935 ) ) ;
#8114 = VECTOR ( 'NONE', #15828, 1000.000000000000227 ) ;
#8115 = ADVANCED_FACE ( 'NONE', ( #11833 ), #18294, .F. ) ;
#8116 = ORIENTED_EDGE ( 'NONE', *, *, #9977, .F. ) ;
#8117 = VERTEX_POINT ( 'NONE', #10220 ) ;
#8118 = VERTEX_POINT ( 'NONE', #13741 ) ;
#8119 = DIRECTION ( 'NONE',  ( 0.5000000000000051070, -0.8660254037844359321, 0.000000000000000000 ) ) ;
#8120 = DIRECTION ( 'NONE',  ( -0.8660254037844362651, -0.5000000000000045519, 5.976026924694053325E-17 ) ) ;
#8121 = FACE_OUTER_BOUND ( 'NONE', #19919, .T. ) ;
#8122 = VECTOR ( 'NONE', #5950, 999.9999999999998863 ) ;
#8123 = CARTESIAN_POINT ( 'NONE',  ( -15.28780296042668141, 58.44014375569393849, -4.952210724505383688 ) ) ;
#8124 = ORIENTED_EDGE ( 'NONE', *, *, #763, .F. ) ;
#8125 = EDGE_CURVE ( 'NONE', #2949, #15199, #8853, .T. ) ;
#8126 = VECTOR ( 'NONE', #5634, 1000.000000000000000 ) ;
#8127 = ORIENTED_EDGE ( 'NONE', *, *, #27, .F. ) ;
#8128 = DIRECTION ( 'NONE',  ( -0.4999999999999995004, 0.8660254037844390407, 0.000000000000000000 ) ) ;
#8129 = AXIS2_PLACEMENT_3D ( 'NONE', #5904, #15894, #15698 ) ;
#8130 = DIRECTION ( 'NONE',  ( -0.8660254037844370423, -0.5000000000000026645, 0.000000000000000000 ) ) ;
#8131 = AXIS2_PLACEMENT_3D ( 'NONE', #8265, #229, #3399 ) ;
#8132 = VECTOR ( 'NONE', #3885, 1000.000000000000000 ) ;
#8133 = CARTESIAN_POINT ( 'NONE',  ( 49.99529059433370293, 237.3619860023655121, 26.00000000000001066 ) ) ;
#8134 = CARTESIAN_POINT ( 'NONE',  ( -28.93295407825220522, 57.46062458779012161, 0.4842793815437907989 ) ) ;
#8135 = CARTESIAN_POINT ( 'NONE',  ( -20.99999999999998224, 15.09941697557068530, 11.45643923738960446 ) ) ;
#8136 = DIRECTION ( 'NONE',  ( -0.5000000000000049960, 0.8660254037844358210, -0.000000000000000000 ) ) ;
#8137 = AXIS2_PLACEMENT_3D ( 'NONE', #19369, #16501, #1879 ) ;
#8138 = CARTESIAN_POINT ( 'NONE',  ( 227.9553588074475670, 39.88513931160575510, -14.00000000000005507 ) ) ;
#8139 = ORIENTED_EDGE ( 'NONE', *, *, #13422, .F. ) ;
#8140 = ORIENTED_EDGE ( 'NONE', *, *, #5666, .F. ) ;
#8141 = CARTESIAN_POINT ( 'NONE',  ( 55.75516069692580601, 77.35848107071853974, -8.459772044266193447 ) ) ;
#8142 = ORIENTED_EDGE ( 'NONE', *, *, #7939, .T. ) ;
#8143 = CARTESIAN_POINT ( 'NONE',  ( -3.344164530110952605, 66.09831342192623538, 2.470462955493161417 ) ) ;
#8144 = CARTESIAN_POINT ( 'NONE',  ( 197.5418782473972499, 4.813505606965178707, -5.993340328401664863 ) ) ;
#8145 = VECTOR ( 'NONE', #16598, 1000.000000000000114 ) ;
#8146 = VECTOR ( 'NONE', #11640, 1000.000000000000000 ) ;
#8147 = ADVANCED_FACE ( 'NONE', ( #16713 ), #12045, .F. ) ;
#8148 = ORIENTED_EDGE ( 'NONE', *, *, #8768, .F. ) ;
#8149 = DIRECTION ( 'NONE',  ( 0.6123724356957914727, 0.3535533905932749521, -0.7071067811865495711 ) ) ;
#8150 = AXIS2_PLACEMENT_3D ( 'NONE', #920, #4410, #5777 ) ;
#8151 = VECTOR ( 'NONE', #19140, 1000.000000000000114 ) ;
#8152 = CARTESIAN_POINT ( 'NONE',  ( 219.5040334327211156, 36.00674583428711628, -10.54439633573327129 ) ) ;
#8153 = ORIENTED_EDGE ( 'NONE', *, *, #1616, .T. ) ;
#8154 = LINE ( 'NONE', #5498, #1334 ) ;
#8155 = DIRECTION ( 'NONE',  ( 1.000000000000000000, -0.000000000000000000, -0.000000000000000000 ) ) ;
#8156 = LINE ( 'NONE', #14668, #5774 ) ;
#8157 = VERTEX_POINT ( 'NONE', #12152 ) ;
#8158 = DIRECTION ( 'NONE',  ( -0.4330127018922214077, -0.2500000000000045519, -0.8660254037844363761 ) ) ;
#8159 = CARTESIAN_POINT ( 'NONE',  ( 199.4425753138606296, -0.2082645440182918917, -20.84195174293567376 ) ) ;
#8160 = DIRECTION ( 'NONE',  ( 0.8660254037844360431, 0.5000000000000044409, -5.976026924694053325E-17 ) ) ;
#8161 = EDGE_CURVE ( 'NONE', #4687, #13750, #14578, .T. ) ;
#8162 = AXIS2_PLACEMENT_3D ( 'NONE', #14293, #19146, #11085 ) ;
#8163 = DIRECTION ( 'NONE',  ( -0.8660254037844380415, -0.5000000000000014433, -0.000000000000000000 ) ) ;
#8164 = CARTESIAN_POINT ( 'NONE',  ( 1.500000000000001332, 0.000000000000000000, 0.000000000000000000 ) ) ;
#8165 = ORIENTED_EDGE ( 'NONE', *, *, #19118, .T. ) ;
#8166 = AXIS2_PLACEMENT_3D ( 'NONE', #8056, #5089, #19413 ) ;
#8167 = EDGE_LOOP ( 'NONE', ( #3633, #19169, #7497, #18001 ) ) ;
#8168 = CIRCLE ( 'NONE', #5453, 4.999999999999989342 ) ;
#8169 = DIRECTION ( 'NONE',  ( 0.8660254037844370423, 0.5000000000000026645, -0.000000000000000000 ) ) ;
#8170 = LINE ( 'NONE', #8060, #16284 ) ;
#8171 = AXIS2_PLACEMENT_3D ( 'NONE', #16790, #2269, #2169 ) ;
#8172 = ORIENTED_EDGE ( 'NONE', *, *, #7208, .T. ) ;
#8173 = CARTESIAN_POINT ( 'NONE',  ( -14.28172431065628523, 71.25647787916724951, -4.698501153746495795 ) ) ;
#8174 = CARTESIAN_POINT ( 'NONE',  ( 78.08475988003900170, 52.31638249278350372, -9.615814618914521716 ) ) ;
#8175 = EDGE_CURVE ( 'NONE', #13077, #11736, #10542, .T. ) ;
#8177 = ORIENTED_EDGE ( 'NONE', *, *, #3839, .T. ) ;
#8176 = VERTEX_POINT ( 'NONE', #2510 ) ;
#8178 = EDGE_CURVE ( 'NONE', #17780, #9666, #8953, .T. ) ;
#8179 = CARTESIAN_POINT ( 'NONE',  ( 28.00000000000001066, 65.00000000000000000, -12.50000000000000000 ) ) ;
#8180 = ORIENTED_EDGE ( 'NONE', *, *, #12536, .F. ) ;
#8181 = CARTESIAN_POINT ( 'NONE',  ( -31.83924231307694441, 66.25779166050591584, 2.455816886943472888 ) ) ;
#8182 = VERTEX_POINT ( 'NONE', #15453 ) ;
#8183 = LINE ( 'NONE', #20904, #7702 ) ;
#8184 = AXIS2_PLACEMENT_3D ( 'NONE', #12096, #7104, #7213 ) ;
#8185 = AXIS2_PLACEMENT_3D ( 'NONE', #5007, #17652, #15963 ) ;
#8186 = CARTESIAN_POINT ( 'NONE',  ( -31.74999999999995737, 0.000000000000000000, 4.000000000000000000 ) ) ;
#8187 = COLOUR_RGB ( '',0.7921568627450980005, 0.8196078431372548767, 0.9333333333333333481 ) ;
#8188 = CARTESIAN_POINT ( 'NONE',  ( 208.9194833127196489, 31.78152281641241572, -14.00000000000007816 ) ) ;
#8189 = CARTESIAN_POINT ( 'NONE',  ( 54.68102985684372896, 77.81511808474795089, -10.30370030985628027 ) ) ;
#8190 = DIRECTION ( 'NONE',  ( 0.5000000000000054401, -0.8660254037844354880, 0.000000000000000000 ) ) ;
#8191 = ORIENTED_EDGE ( 'NONE', *, *, #20007, .F. ) ;
#8192 = FACE_OUTER_BOUND ( 'NONE', #1665, .T. ) ;
#8193 = ORIENTED_EDGE ( 'NONE', *, *, #17197, .T. ) ;
#8194 = FACE_OUTER_BOUND ( 'NONE', #17159, .T. ) ;
#8195 = B_SPLINE_CURVE_WITH_KNOTS ( 'NONE', 3,
 ( #17190, #19935, #7418, #12211 ),
 .UNSPECIFIED., .F., .F.,
 ( 4, 4 ),
 ( 4.589663078223623554E-07, 0.0006731097583619476436 ),
 .UNSPECIFIED. ) ;
#8196 = ADVANCED_FACE ( 'NONE', ( #5874 ), #12576, .F. ) ;
#8197 = ORIENTED_EDGE ( 'NONE', *, *, #7183, .F. ) ;
#8198 = EDGE_CURVE ( 'NONE', #8802, #7294, #1131, .T. ) ;
#8199 = CARTESIAN_POINT ( 'NONE',  ( 211.4194833127196489, 27.45139579749023540, -14.00000000000004974 ) ) ;
#8200 = CARTESIAN_POINT ( 'NONE',  ( 69.50490953756755630, 173.5703347563769796, 11.00000000000001243 ) ) ;
#8201 = CARTESIAN_POINT ( 'NONE',  ( 188.4110409874304253, 14.81153516656304880, -14.00000000000005507 ) ) ;
#8202 = CARTESIAN_POINT ( 'NONE',  ( 218.9922241104002012, 10.30591036058324583, -12.64773574313060678 ) ) ;
#8203 = FACE_OUTER_BOUND ( 'NONE', #10281, .T. ) ;
#8204 = CARTESIAN_POINT ( 'NONE',  ( 218.6961259033436988, 38.05395589839552173, -11.55788255683058807 ) ) ;
#8205 = EDGE_LOOP ( 'NONE', ( #12074, #18255, #3856, #8494 ) ) ;
#8206 = EDGE_CURVE ( 'NONE', #19279, #4064, #1439, .T. ) ;
#8207 = CARTESIAN_POINT ( 'NONE',  ( 70.65802621385911664, 70.89520902279555514, -24.10184437820831960 ) ) ;
#8208 = CARTESIAN_POINT ( 'NONE',  ( -10.07778552363583380, 45.21291330008718745, -11.01476690536905956 ) ) ;
#8209 = CIRCLE ( 'NONE', #16028, 0.004059536337672174817 ) ;
#8210 = ORIENTED_EDGE ( 'NONE', *, *, #20794, .T. ) ;
#8211 = DIRECTION ( 'NONE',  ( 0.8660254037844360431, 0.5000000000000044409, -5.976026924694052093E-17 ) ) ;
#8212 = CARTESIAN_POINT ( 'NONE',  ( -4.250339552839886181, 57.32441097052598877, 4.267670548753550008 ) ) ;
#8213 = CARTESIAN_POINT ( 'NONE',  ( 38.17255043510031953, 120.8395726428435637, -12.49999999999999822 ) ) ;
#8214 = EDGE_CURVE ( 'NONE', #10554, #7321, #17342, .T. ) ;
#8215 = CARTESIAN_POINT ( 'NONE',  ( 213.3673372177917997, 7.058380398974537506, -1.942038651984889785 ) ) ;
#8216 = CARTESIAN_POINT ( 'NONE',  ( -31.74999999999995737, 0.000000000000000000, 0.000000000000000000 ) ) ;
#8218 = VERTEX_POINT ( 'NONE', #15971 ) ;
#8217 = ORIENTED_EDGE ( 'NONE', *, *, #2685, .T. ) ;
#8219 = VERTEX_POINT ( 'NONE', #18724 ) ;
#8220 = FACE_OUTER_BOUND ( 'NONE', #20198, .T. ) ;
#8221 = PLANE ( 'NONE',  #2408 ) ;
#8222 = EDGE_CURVE ( 'NONE', #7280, #14632, #20404, .T. ) ;
#8223 = ORIENTED_EDGE ( 'NONE', *, *, #11804, .F. ) ;
#8224 = ORIENTED_EDGE ( 'NONE', *, *, #18518, .F. ) ;
#8225 = CARTESIAN_POINT ( 'NONE',  ( -19.29903332301958585, 60.14018031781252205, -3.758841495318848480 ) ) ;
#8226 = DIRECTION ( 'NONE',  ( 0.000000000000000000, 6.938893903907178303E-18, 1.000000000000000000 ) ) ;
#8227 = CARTESIAN_POINT ( 'NONE',  ( 209.8577037357181894, 2.614299844655262106, -14.00000000000005507 ) ) ;
#8228 = FACE_OUTER_BOUND ( 'NONE', #18540, .T. ) ;
#8229 = AXIS2_PLACEMENT_3D ( 'NONE', #8320, #6719, #3554 ) ;
#8230 = ORIENTED_EDGE ( 'NONE', *, *, #1187, .F. ) ;
#8231 = ORIENTED_EDGE ( 'NONE', *, *, #11612, .T. ) ;
#8232 = LINE ( 'NONE', #11328, #8705 ) ;
#8233 = EDGE_CURVE ( 'NONE', #140, #7292, #14286, .T. ) ;
#8234 = EDGE_CURVE ( 'NONE', #7840, #2330, #11867, .T. ) ;
#8235 = CARTESIAN_POINT ( 'NONE',  ( 220.7941474011230127, 33.80222769952564477, -17.14987233279968848 ) ) ;
#8236 = FACE_OUTER_BOUND ( 'NONE', #6463, .T. ) ;
#8237 = CARTESIAN_POINT ( 'NONE',  ( -28.84012200976501461, 59.46807757785196458, 1.471601637521282591 ) ) ;
#8238 = CARTESIAN_POINT ( 'NONE',  ( 199.3200586684138784, -0.7942204290835060965, -8.555339712719925771 ) ) ;
#8239 = VECTOR ( 'NONE', #18234, 1000.000000000000227 ) ;
#8240 =( REPRESENTATION_RELATIONSHIP ('NONE','NONE', #4634, #6911 ) REPRESENTATION_RELATIONSHIP_WITH_TRANSFORMATION ( #20873 )SHAPE_REPRESENTATION_RELATIONSHIP( ) );
#8241 = AXIS2_PLACEMENT_3D ( 'NONE', #859, #18982, #5709 ) ;
#8242 = EDGE_CURVE ( 'NONE', #11211, #18235, #14268, .T. ) ;
#8243 = VERTEX_POINT ( 'NONE', #17551 ) ;
#8244 = CARTESIAN_POINT ( 'NONE',  ( 198.0727098700125168, 9.775028566371592120, -25.36561010639676184 ) ) ;
#8245 = FACE_OUTER_BOUND ( 'NONE', #3332, .T. ) ;
#8246 = ORIENTED_EDGE ( 'NONE', *, *, #5886, .T. ) ;
#8247 = CARTESIAN_POINT ( 'NONE',  ( 66.25714559803427051, 75.99906101403284708, -4.941591886955796653 ) ) ;
#8248 = ORIENTED_EDGE ( 'NONE', *, *, #8809, .T. ) ;
#8249 = CARTESIAN_POINT ( 'NONE',  ( 218.9522255890561553, 10.79802344239516998, -11.16899820387762432 ) ) ;
#8250 = LINE ( 'NONE', #19806, #546 ) ;
#8251 = EDGE_CURVE ( 'NONE', #13321, #5971, #15980, .T. ) ;
#8252 = B_SPLINE_CURVE_WITH_KNOTS ( 'NONE', 3,
 ( #12092, #4559, #17802, #11025 ),
 .UNSPECIFIED., .F., .F.,
 ( 4, 4 ),
 ( 3.849233602941101093E-07, 0.0005858732790999125533 ),
 .UNSPECIFIED. ) ;
#8253 = ORIENTED_EDGE ( 'NONE', *, *, #919, .F. ) ;
#8254 = FACE_BOUND ( 'NONE', #20644, .T. ) ;
#8255 = EDGE_LOOP ( 'NONE', ( #5563, #5425 ) ) ;
#8256 = AXIS2_PLACEMENT_3D ( 'NONE', #7620, #7513, #955 ) ;
#8257 = DIRECTION ( 'NONE',  ( 0.5000000000000053291, -0.8660254037844355990, -3.330669073875468142E-16 ) ) ;
#8258 = ORIENTED_EDGE ( 'NONE', *, *, #20082, .T. ) ;
#8259 = CARTESIAN_POINT ( 'NONE',  ( 37.85427444295662269, 178.3908428320656299, 11.00000000000001243 ) ) ;
#8260 = DIRECTION ( 'NONE',  ( 0.5000000000000046629, -0.8660254037844360431, -4.006172263299081054E-16 ) ) ;
#8261 = VERTEX_POINT ( 'NONE', #3023 ) ;
#8262 = CARTESIAN_POINT ( 'NONE',  ( 229.7512887155055239, 36.77449746401691044, -13.55260094074461819 ) ) ;
#8263 = CARTESIAN_POINT ( 'NONE',  ( 226.8903291562342588, 40.75035888801145489, -17.68583624946726474 ) ) ;
#8264 = ORIENTED_EDGE ( 'NONE', *, *, #12215, .F. ) ;
#8265 = CARTESIAN_POINT ( 'NONE',  ( 105.1989074543211728, 189.2062061502930135, 11.00000000000001066 ) ) ;
#8266 = DIRECTION ( 'NONE',  ( 0.4999999999999995004, -0.8660254037844390407, 0.000000000000000000 ) ) ;
#8267 = VERTEX_POINT ( 'NONE', #20722 ) ;
#8268 = AXIS2_PLACEMENT_3D ( 'NONE', #6070, #8944, #9249 ) ;
#8269 = DIRECTION ( 'NONE',  ( -0.5000000000000054401, 0.8660254037844354880, -0.000000000000000000 ) ) ;
#8270 = CARTESIAN_POINT ( 'NONE',  ( 81.06335414937042572, 67.01023635845230331, 0.5981178230952700625 ) ) ;
#8271 = ORIENTED_EDGE ( 'NONE', *, *, #13981, .F. ) ;
#8272 = CARTESIAN_POINT ( 'NONE',  ( 61.99529059433385925, 216.5773763115390125, -22.00000000000000355 ) ) ;
#8273 = CARTESIAN_POINT ( 'NONE',  ( 75.61984849132328179, 52.78225778306437377, -16.94885618148015993 ) ) ;
#8275 = EDGE_LOOP ( 'NONE', ( #3462, #2591, #12397, #1775 ) ) ;
#8274 = ORIENTED_EDGE ( 'NONE', *, *, #17841, .F. ) ;
#8276 = VERTEX_POINT ( 'NONE', #6191 ) ;
#8277 = UNCERTAINTY_MEASURE_WITH_UNIT (LENGTH_MEASURE( 1.000000000000000082E-05 ), #15806, 'distance_accuracy_value', 'NONE');
#8278 = ORIENTED_EDGE ( 'NONE', *, *, #13805, .T. ) ;
#8279 = DIRECTION ( 'NONE',  ( 0.5000000000000045519, -0.8660254037844360431, -0.000000000000000000 ) ) ;
#8280 = VERTEX_POINT ( 'NONE', #15559 ) ;
#8281 = CARTESIAN_POINT ( 'NONE',  ( 196.7929107858857094, 4.381089041447214782, -20.84195174293567376 ) ) ;
#8282 = CARTESIAN_POINT ( 'NONE',  ( -32.60712961159122614, 78.11617769706940351, -5.220046598459701315 ) ) ;
#8283 = DIRECTION ( 'NONE',  ( 1.000000000000000000, 0.000000000000000000, 0.000000000000000000 ) ) ;
#8284 = CARTESIAN_POINT ( 'NONE',  ( 221.3208164193364951, 32.89001020120745267, -16.29291827778590118 ) ) ;
#8285 = EDGE_LOOP ( 'NONE', ( #20903, #12020, #4062, #1422 ) ) ;
#8286 = AXIS2_PLACEMENT_3D ( 'NONE', #1814, #2233, #5389 ) ;
#8287 = PLANE ( 'NONE',  #8526 ) ;
#8288 = CIRCLE ( 'NONE', #1695, 12.47473710546057823 ) ;
#8289 = CARTESIAN_POINT ( 'NONE',  ( 72.49529059433407951, 198.3908428320658288, 11.00000000000001066 ) ) ;
#8290 = EDGE_CURVE ( 'NONE', #7763, #15950, #13162, .T. ) ;
#8291 = LINE ( 'NONE', #11599, #11107 ) ;
#8292 = ORIENTED_EDGE ( 'NONE', *, *, #8050, .T. ) ;
#8293 = DIRECTION ( 'NONE',  ( -0.4999999999999995004, 0.8660254037844390407, 0.000000000000000000 ) ) ;
#8294 = DIRECTION ( 'NONE',  ( -0.4988343845952724065, 0.8640064986813599246, 0.06824241336466067842 ) ) ;
#8295 = ORIENTED_EDGE ( 'NONE', *, *, #2740, .F. ) ;
#8296 = AXIS2_PLACEMENT_3D ( 'NONE', #18735, #18838, #5986 ) ;
#8297 = CYLINDRICAL_SURFACE ( 'NONE', #11559, 3.902363844300889451 ) ;
#8299 = VERTEX_POINT ( 'NONE', #9468 ) ;
#8298 = VERTEX_POINT ( 'NONE', #19138 ) ;
#8300 = AXIS2_PLACEMENT_3D ( 'NONE', #12, #13359, #18123 ) ;
#8301 = DIRECTION ( 'NONE',  ( 0.8660254037844355990, 0.5000000000000054401, 0.000000000000000000 ) ) ;
#8302 = CARTESIAN_POINT ( 'NONE',  ( 215.4747034159835550, 15.16702704537912183, -19.61257667712965258 ) ) ;
#8303 = AXIS2_PLACEMENT_3D ( 'NONE', #9101, #7518, #10917 ) ;
#8304 = DIRECTION ( 'NONE',  ( 0.8660254037844361541, 0.5000000000000044409, -5.976026924694052093E-17 ) ) ;
#8305 = ADVANCED_FACE ( 'NONE', ( #20298, #17444 ), #5766, .F. ) ;
#8306 = CARTESIAN_POINT ( 'NONE',  ( 204.5452479762167002, 2.222544024343242608, -2.867675856073625518 ) ) ;
#8307 = CARTESIAN_POINT ( 'NONE',  ( -30.00000000000002842, 4.999999999999995559, -8.933394465404589369 ) ) ;
#8308 = PLANE ( 'NONE',  #10988 ) ;
#8309 = ORIENTED_EDGE ( 'NONE', *, *, #4314, .T. ) ;
#8310 = B_SPLINE_CURVE_WITH_KNOTS ( 'NONE', 3,
 ( #4310, #2931, #9372, #14076 ),
 .UNSPECIFIED., .F., .F.,
 ( 4, 4 ),
 ( 2.816680711552148146E-07, 0.0006729324601260043559 ),
 .UNSPECIFIED. ) ;
#8311 = DIRECTION ( 'NONE',  ( -0.8660254037844359321, -0.5000000000000045519, 5.976026924694053325E-17 ) ) ;
#8312 = CIRCLE ( 'NONE', #19817, 3.619616396367202782 ) ;
#8313 = CARTESIAN_POINT ( 'NONE',  ( -3.625355398317132494, 51.79533773540889285, 1.819264427481864121 ) ) ;
#8314 = EDGE_CURVE ( 'NONE', #9110, #11936, #2545, .T. ) ;
#8315 = ORIENTED_EDGE ( 'NONE', *, *, #15986, .F. ) ;
#8316 = AXIS2_PLACEMENT_3D ( 'NONE', #17791, #3263, #9715 ) ;
#8317 = EDGE_CURVE ( 'NONE', #13220, #4359, #9469, .T. ) ;
#8318 = CARTESIAN_POINT ( 'NONE',  ( 215.2040058117673595, 19.66578688991103974, -14.05525385477321620 ) ) ;
#8319 = CARTESIAN_POINT ( 'NONE',  ( -3.548890045384964331, 48.22447992834113251, -1.142799159744782411 ) ) ;
#8320 = CARTESIAN_POINT ( 'NONE',  ( 4.000000000000000000, 0.000000000000000000, 0.000000000000000000 ) ) ;
#8321 = VECTOR ( 'NONE', #3682, 1000.000000000000000 ) ;
#8322 = CARTESIAN_POINT ( 'NONE',  ( -15.99999999999999289, 20.09941697557067997, 4.999999999999989342 ) ) ;
#8323 = CARTESIAN_POINT ( 'NONE',  ( 16.51452848080062097, 235.3523670591319217, -19.00000000000000355 ) ) ;
#8325 = EDGE_LOOP ( 'NONE', ( #5734, #7116, #20844, #4995 ) ) ;
#8324 = ORIENTED_EDGE ( 'NONE', *, *, #19129, .F. ) ;
#8326 = ORIENTED_EDGE ( 'NONE', *, *, #10396, .F. ) ;
#8327 = ORIENTED_EDGE ( 'NONE', *, *, #19951, .T. ) ;
#8328 = LINE ( 'NONE', #3564, #4760 ) ;
#8329 = DIRECTION ( 'NONE',  ( 0.000000000000000000, 0.000000000000000000, -1.000000000000000000 ) ) ;
#8330 = EDGE_LOOP ( 'NONE', ( #19170, #13459, #312, #14094, #15891, #12655, #14236, #3831 ) ) ;
#8331 = ORIENTED_EDGE ( 'NONE', *, *, #1068, .F. ) ;
#8332 = ADVANCED_FACE ( 'NONE', ( #7467 ), #18824, .F. ) ;
#8333 = CARTESIAN_POINT ( 'NONE',  ( -16.71639762958279007, 58.44083456968236590, -4.951609446663259639 ) ) ;
#8334 = DIRECTION ( 'NONE',  ( -1.000000000000000000, -0.000000000000000000, -0.000000000000000000 ) ) ;
#8335 = DIRECTION ( 'NONE',  ( 0.8660254037844380415, 0.5000000000000014433, 0.000000000000000000 ) ) ;
#8336 = VECTOR ( 'NONE', #9248, 1000.000000000000114 ) ;
#8337 = CARTESIAN_POINT ( 'NONE',  ( -14.27770786790704705, 58.73247755281146709, -4.704935945893314653 ) ) ;
#8338 = EDGE_LOOP ( 'NONE', ( #19745, #15873 ) ) ;
#8339 = VERTEX_POINT ( 'NONE', #14176 ) ;
#8340 = CIRCLE ( 'NONE', #20519, 12.47473710546057823 ) ;
#8341 = PLANE ( 'NONE',  #4313 ) ;
#8342 = ADVANCED_FACE ( 'NONE', ( #6079 ), #14065, .F. ) ;
#8343 = ORIENTED_EDGE ( 'NONE', *, *, #16651, .F. ) ;
#8344 = FACE_BOUND ( 'NONE', #17345, .T. ) ;
#8345 = EDGE_CURVE ( 'NONE', #3730, #4124, #7988, .T. ) ;
#8346 = DIRECTION ( 'NONE',  ( 0.6299240516454519545, 0.3636868207865264768, -0.6862416378687370422 ) ) ;
#8347 = CARTESIAN_POINT ( 'NONE',  ( -28.16085501120128853, 46.85610706404197146, -2.909190404198925162 ) ) ;
#8348 = DIRECTION ( 'NONE',  ( -0.5000000000000054401, 0.8660254037844354880, -0.000000000000000000 ) ) ;
#8349 = ADVANCED_FACE ( 'NONE', ( #254 ), #9780, .F. ) ;
#8350 = FACE_OUTER_BOUND ( 'NONE', #2643, .T. ) ;
#8351 = CARTESIAN_POINT ( 'NONE',  ( 61.99529059433385925, 216.5773763115390125, -22.00000000000000355 ) ) ;
#8352 = CIRCLE ( 'NONE', #18170, 5.000000000000005329 ) ;
#8353 = ORIENTED_EDGE ( 'NONE', *, *, #5613, .F. ) ;
#8354 = ORIENTED_EDGE ( 'NONE', *, *, #1647, .T. ) ;
#8355 = CARTESIAN_POINT ( 'NONE',  ( 69.95688439207881970, 76.67563175530182207, -1.651812347404341796 ) ) ;
#8356 = ADVANCED_FACE ( 'NONE', ( #19343 ), #18069, .F. ) ;
#8357 = ORIENTED_EDGE ( 'NONE', *, *, #19788, .T. ) ;
#8358 = EDGE_CURVE ( 'NONE', #11939, #8182, #9113, .T. ) ;
#8359 = VERTEX_POINT ( 'NONE', #16076 ) ;
#8360 = LINE ( 'NONE', #212, #3081 ) ;
#8361 = ORIENTED_EDGE ( 'NONE', *, *, #17468, .T. ) ;
#8362 = DIRECTION ( 'NONE',  ( 0.8660254037844355990, 0.5000000000000054401, 0.000000000000000000 ) ) ;
#8363 = ADVANCED_FACE ( 'NONE', ( #6699 ), #19434, .F. ) ;
#8364 = LINE ( 'NONE', #2020, #8239 ) ;
#8365 = VERTEX_POINT ( 'NONE', #11489 ) ;
#8366 = VECTOR ( 'NONE', #18867, 1000.000000000000114 ) ;
#8367 = DIRECTION ( 'NONE',  ( 0.8660254037844360431, 0.5000000000000044409, -5.976026924694053325E-17 ) ) ;
#8368 = DIRECTION ( 'NONE',  ( -0.5000000000000051070, 0.8660254037844359321, -0.000000000000000000 ) ) ;
#8369 = VECTOR ( 'NONE', #6812, 1000.000000000000114 ) ;
#8370 = DIRECTION ( 'NONE',  ( -0.8660254037844378194, -0.5000000000000013323, -0.000000000000000000 ) ) ;
#8371 = DIRECTION ( 'NONE',  ( -0.4439426092011903302, 0.7689311547811512604, 0.4600650377311499839 ) ) ;
#8372 = EDGE_CURVE ( 'NONE', #15566, #3379, #16266, .T. ) ;
#8373 = ORIENTED_EDGE ( 'NONE', *, *, #15859, .F. ) ;
#8374 = CARTESIAN_POINT ( 'NONE',  ( 48.16104799571871098, 210.5389873765740560, 45.89527237623691747 ) ) ;
#8375 = CARTESIAN_POINT ( 'NONE',  ( -14.99999999999999822, 0.000000000000000000, -28.99999999999999645 ) ) ;
#8376 = CARTESIAN_POINT ( 'NONE',  ( 215.9002224801550085, 8.520742387026412956, -22.69908973750352743 ) ) ;
#8377 = VERTEX_POINT ( 'NONE', #9978 ) ;
#8378 = FACE_OUTER_BOUND ( 'NONE', #17806, .T. ) ;
#8379 = ADVANCED_FACE ( 'NONE', ( #8192 ), #55, .F. ) ;
#8380 = CARTESIAN_POINT ( 'NONE',  ( 202.5824069535873662, 24.78489278575215238, -12.54844597431177178 ) ) ;
#8381 = CIRCLE ( 'NONE', #608, 5.000000000000000888 ) ;
#8382 = CARTESIAN_POINT ( 'NONE',  ( 211.5875185857062206, 6.803621723274593691, -25.94618751764496878 ) ) ;
#8383 = CARTESIAN_POINT ( 'NONE',  ( 76.24641241968245708, 53.61856141616145521, -6.137685929381720307 ) ) ;
#8384 = B_SPLINE_CURVE_WITH_KNOTS ( 'NONE', 3,
 ( #7789, #9069, #14294, #15569 ),
 .UNSPECIFIED., .F., .F.,
 ( 4, 4 ),
 ( 4.749816698181874535E-07, 0.0004525282234497410793 ),
 .UNSPECIFIED. ) ;
#8385 = VECTOR ( 'NONE', #20340, 1000.000000000000000 ) ;
#8387 = VERTEX_POINT ( 'NONE', #14701 ) ;
#8386 = EDGE_LOOP ( 'NONE', ( #15865, #5191, #13368, #15928 ) ) ;
#8388 = ORIENTED_EDGE ( 'NONE', *, *, #8831, .F. ) ;
#8389 = CARTESIAN_POINT ( 'NONE',  ( 226.2060741798980246, 42.26203003091832500, -16.42873025640173523 ) ) ;
#8390 = ORIENTED_EDGE ( 'NONE', *, *, #9413, .F. ) ;
#8391 = CARTESIAN_POINT ( 'NONE',  ( 75.73459986189040194, 52.93517924382847895, -17.35279103460518968 ) ) ;
#8392 = CARTESIAN_POINT ( 'NONE',  ( -23.11077747421012063, 79.96752057144479409, -11.48167302094428344 ) ) ;
#8393 = LINE ( 'NONE', #14896, #3219 ) ;
#8394 = DIRECTION ( 'NONE',  ( 0.5000000000000027756, -0.8660254037844372643, 0.000000000000000000 ) ) ;
#8395 = MECHANICAL_DESIGN_GEOMETRIC_PRESENTATION_REPRESENTATION (  '', ( #5327 ), #3644 ) ;
#8396 = CARTESIAN_POINT ( 'NONE',  ( 219.3291089353582493, 36.33974875727300002, -10.64970491435233058 ) ) ;
#8397 = AXIS2_PLACEMENT_3D ( 'NONE', #10493, #18467, #10385 ) ;
#8398 = SHAPE_REPRESENTATION ( 'socket head cap screw_iso_ISO 4762 M10 x 16 - 16N', ( #18233 ), #11452 ) ;
#8399 = CARTESIAN_POINT ( 'NONE',  ( 67.54734661231900361, 72.27942328892467572, -1.687414245825497261 ) ) ;
#8400 = CARTESIAN_POINT ( 'NONE',  ( 195.4677224586705222, 19.39634291273559086, -14.00000000000005329 ) ) ;
#8401 = ORIENTED_EDGE ( 'NONE', *, *, #7916, .F. ) ;
#8402 = CYLINDRICAL_SURFACE ( 'NONE', #10480, 13.99999999999999822 ) ;
#8403 = DIRECTION ( 'NONE',  ( 0.000000000000000000, 0.000000000000000000, -1.000000000000000000 ) ) ;
#8404 = ORIENTED_EDGE ( 'NONE', *, *, #20514, .F. ) ;
#8405 = DIRECTION ( 'NONE',  ( 0.000000000000000000, 0.000000000000000000, -1.000000000000000000 ) ) ;
#8406 = ORIENTED_EDGE ( 'NONE', *, *, #19776, .T. ) ;
#8407 = VECTOR ( 'NONE', #10613, 1000.000000000000000 ) ;
#8408 = CARTESIAN_POINT ( 'NONE',  ( 192.7739465146478040, 17.33045984715094434, -24.01557619556968248 ) ) ;
#8409 = CARTESIAN_POINT ( 'NONE',  ( 0.000000000000000000, 8.375619485785039961E-16, -6.500000000000000888 ) ) ;
#8410 = CARTESIAN_POINT ( 'NONE',  ( 226.2951554528370934, 42.76069587268737848, -11.94979443502191963 ) ) ;
#8411 = CARTESIAN_POINT ( 'NONE',  ( 81.83695616705894338, 65.97962712285851694, -25.63559049685116165 ) ) ;
#8412 = EDGE_CURVE ( 'NONE', #15359, #3430, #20842, .T. ) ;
#8413 = CARTESIAN_POINT ( 'NONE',  ( -26.22872419829098334, 5.421422414486862351, -7.194700298646708347 ) ) ;
#8414 = CARTESIAN_POINT ( 'NONE',  ( 214.5005434568852820, 19.25964270995510930, -9.448537646917806399 ) ) ;
#8415 = ORIENTED_EDGE ( 'NONE', *, *, #10924, .T. ) ;
#8416 = CARTESIAN_POINT ( 'NONE',  ( 77.64566045588958332, 55.52805080504859347, -21.41780359453167293 ) ) ;
#8417 = CARTESIAN_POINT ( 'NONE',  ( -8.151266174553969179, 45.02035806555345943, -9.759823581491495759 ) ) ;
#8418 = VECTOR ( 'NONE', #1374, 1000.000000000000227 ) ;
#8419 = ORIENTED_EDGE ( 'NONE', *, *, #4324, .T. ) ;
#8420 = DIRECTION ( 'NONE',  ( 0.8660254037844352659, 0.5000000000000056621, 0.000000000000000000 ) ) ;
#8421 = CARTESIAN_POINT ( 'NONE',  ( -3.954476518211411662, 54.76190936792474417, 3.362518328805365719 ) ) ;
#8422 = DIRECTION ( 'NONE',  ( -1.000000000000000000, -0.000000000000000000, -0.000000000000000000 ) ) ;
#8423 = CARTESIAN_POINT ( 'NONE',  ( 227.9553588074475954, 39.88513931160571957, -14.00000000000005507 ) ) ;
#8424 = CARTESIAN_POINT ( 'NONE',  ( 211.6495311407713018, 17.61360998178372483, -6.376588578941996488 ) ) ;
#8425 = EDGE_CURVE ( 'NONE', #7321, #4222, #2390, .T. ) ;
#8426 = DIRECTION ( 'NONE',  ( 0.000000000000000000, 0.000000000000000000, 1.000000000000000000 ) ) ;
#8428 = ORIENTED_EDGE ( 'NONE', *, *, #3950, .F. ) ;
#8427 = ORIENTED_EDGE ( 'NONE', *, *, #12346, .T. ) ;
#8429 = ORIENTED_EDGE ( 'NONE', *, *, #8594, .T. ) ;
#8430 = ORIENTED_EDGE ( 'NONE', *, *, #6429, .T. ) ;
#8431 = DIRECTION ( 'NONE',  ( 1.000000000000000000, 0.000000000000000000, 0.000000000000000000 ) ) ;
#8432 = DIRECTION ( 'NONE',  ( 0.000000000000000000, 0.000000000000000000, 1.000000000000000000 ) ) ;
#8433 = ORIENTED_EDGE ( 'NONE', *, *, #12719, .F. ) ;
#8434 = ORIENTED_EDGE ( 'NONE', *, *, #18496, .T. ) ;
#8435 = DIRECTION ( 'NONE',  ( -0.5000000000000043299, 0.8660254037844361541, 1.067522139062650548E-16 ) ) ;
#8436 = CARTESIAN_POINT ( 'NONE',  ( 225.8286226823958884, 43.56875433448772839, -13.99751724578379708 ) ) ;
#8437 = CARTESIAN_POINT ( 'NONE',  ( 85.37797649651368204, 230.0773763115391262, 1.000000000000017097 ) ) ;
#8438 = ORIENTED_EDGE ( 'NONE', *, *, #6417, .T. ) ;
#8439 = EDGE_CURVE ( 'NONE', #15581, #10176, #7445, .T. ) ;
#8440 = DIRECTION ( 'NONE',  ( 0.000000000000000000, -1.000000000000000000, 0.000000000000000000 ) ) ;
#8441 = EDGE_CURVE ( 'NONE', #11248, #13321, #14389, .T. ) ;
#8442 = CARTESIAN_POINT ( 'NONE',  ( -31.74999999999995737, 0.000000000000000000, 0.000000000000000000 ) ) ;
#8443 = CIRCLE ( 'NONE', #20295, 11.98469917212512215 ) ;
#8444 = ORIENTED_EDGE ( 'NONE', *, *, #7317, .T. ) ;
#8445 = VECTOR ( 'NONE', #3044, 999.9999999999998863 ) ;
#8446 = CYLINDRICAL_SURFACE ( 'NONE', #20291, 2.499999999999994671 ) ;
#8447 = CIRCLE ( 'NONE', #13541, 15.00000000000001954 ) ;
#8448 = PLANE ( 'NONE',  #11930 ) ;
#8449 = CARTESIAN_POINT ( 'NONE',  ( -28.47807888696556589, 50.32121178641160242, 0.7806563195649840470 ) ) ;
#8450 = CARTESIAN_POINT ( 'NONE',  ( 49.01452848080091229, 179.0607158131434176, 26.00000000000001776 ) ) ;
#8451 = FACE_OUTER_BOUND ( 'NONE', #4723, .T. ) ;
#8452 = DIRECTION ( 'NONE',  ( -1.000000000000000000, 0.000000000000000000, 0.000000000000000000 ) ) ;
#8453 = PRODUCT_RELATED_PRODUCT_CATEGORY ( 'part', '', ( #20237 ) ) ;
#8454 = ORIENTED_EDGE ( 'NONE', *, *, #2150, .F. ) ;
#8456 = EDGE_CURVE ( 'NONE', #18828, #5642, #20815, .T. ) ;
#8455 = CARTESIAN_POINT ( 'NONE',  ( 62.45904372457708575, 78.26118437974417930, -12.42744951105453488 ) ) ;
#8457 = AXIS2_PLACEMENT_3D ( 'NONE', #4514, #20502, #7886 ) ;
#8458 = ORIENTED_EDGE ( 'NONE', *, *, #6555, .T. ) ;
#8459 = ORIENTED_EDGE ( 'NONE', *, *, #15118, .T. ) ;
#8460 = ORIENTED_EDGE ( 'NONE', *, *, #1995, .F. ) ;
#8461 = DIRECTION ( 'NONE',  ( 0.000000000000000000, 0.000000000000000000, -1.000000000000000000 ) ) ;
#8462 = FACE_OUTER_BOUND ( 'NONE', #5386, .T. ) ;
#8463 = B_SPLINE_CURVE_WITH_KNOTS ( 'NONE', 3,
 ( #16676, #6689, #8608, #18059 ),
 .UNSPECIFIED., .F., .F.,
 ( 4, 4 ),
 ( 5.020066588617606599E-07, 0.0005859903623984905486 ),
 .UNSPECIFIED. ) ;
#8464 = EDGE_CURVE ( 'NONE', #11761, #9937, #1809, .T. ) ;
#8465 = ORIENTED_EDGE ( 'NONE', *, *, #14702, .F. ) ;
#8466 = CARTESIAN_POINT ( 'NONE',  ( 220.1316027948978729, 34.91976381372831639, -17.54145750504260093 ) ) ;
#8467 = VECTOR ( 'NONE', #15089, 1000.000000000000114 ) ;
#8468 = CARTESIAN_POINT ( 'NONE',  ( 227.9553588074475670, 39.88513931160575510, -14.00000000000005507 ) ) ;
#8469 = EDGE_LOOP ( 'NONE', ( #4333, #17155, #16248, #20102, #8458 ) ) ;
#8470 = CARTESIAN_POINT ( 'NONE',  ( 220.5324068401904754, 32.74206926103874338, -16.57782486433073998 ) ) ;
#8471 = DIRECTION ( 'NONE',  ( -0.5000000000000006661, 1.000482654775420499E-16, -0.8660254037844382635 ) ) ;
#8472 = EDGE_CURVE ( 'NONE', #13077, #9607, #3392, .T. ) ;
#8473 = AXIS2_PLACEMENT_3D ( 'NONE', #3613, #10671, #10065 ) ;
#8474 = ADVANCED_FACE ( 'NONE', ( #17760 ), #9681, .F. ) ;
#8475 = DIRECTION ( 'NONE',  ( -0.4999999999999995004, 0.8660254037844390407, 0.000000000000000000 ) ) ;
#8476 = CARTESIAN_POINT ( 'NONE',  ( 226.0041978322375087, 43.26464925441552367, -12.30768923015393490 ) ) ;
#8477 = VECTOR ( 'NONE', #1885, 1000.000000000000114 ) ;
#8478 = ORIENTED_EDGE ( 'NONE', *, *, #14298, .F. ) ;
#8479 = DIRECTION ( 'NONE',  ( 0.7499999999999954481, 0.4330127018922224624, -0.5000000000000038858 ) ) ;
#8480 = DIRECTION ( 'NONE',  ( 0.5000000000000052180, -0.8660254037844355990, 8.326672684688672821E-17 ) ) ;
#8481 = PLANE ( 'NONE',  #1097 ) ;
#8482 = ORIENTED_EDGE ( 'NONE', *, *, #14081, .F. ) ;
#8484 = EDGE_CURVE ( 'NONE', #19224, #15281, #10840, .T. ) ;
#8483 = CARTESIAN_POINT ( 'NONE',  ( 77.00490953756757051, 160.5799536996104564, 56.00000000000000711 ) ) ;
#8485 = VECTOR ( 'NONE', #18400, 1000.000000000000000 ) ;
#8486 = CARTESIAN_POINT ( 'NONE',  ( 203.2866962553531778, 23.96679637293826204, -13.60843650710557462 ) ) ;
#8487 = AXIS2_PLACEMENT_3D ( 'NONE', #1505, #20881, #6357 ) ;
#8488 = CARTESIAN_POINT ( 'NONE',  ( -12.98588573640857291, 70.25594724513304357, -3.991311237440293258 ) ) ;
#8489 = VECTOR ( 'NONE', #1615, 1000.000000000000114 ) ;
#8490 = AXIS2_PLACEMENT_3D ( 'NONE', #3664, #10010, #18300 ) ;
#8491 = CARTESIAN_POINT ( 'NONE',  ( 75.38193994203784598, 52.46588049713438551, -15.95886351416976900 ) ) ;
#8492 = EDGE_CURVE ( 'NONE', #15613, #17576, #1370, .T. ) ;
#8494 = ORIENTED_EDGE ( 'NONE', *, *, #19362, .F. ) ;
#8493 = VERTEX_POINT ( 'NONE', #18169 ) ;
#8495 = CONICAL_SURFACE ( 'NONE', #19337, 4.509097725792825528, 0.5235987755983015912 ) ;
#8496 = ORIENTED_EDGE ( 'NONE', *, *, #17956, .F. ) ;
#8497 = VECTOR ( 'NONE', #4850, 1000.000000000000227 ) ;
#8498 = DIRECTION ( 'NONE',  ( -0.5000000000000034417, 1.060575238724904696E-16, -0.8660254037844367092 ) ) ;
#8499 = ORIENTED_EDGE ( 'NONE', *, *, #3494, .F. ) ;
#8500 = CARTESIAN_POINT ( 'NONE',  ( 75.05058039824011473, 52.02675804008249827, -13.40131898612561301 ) ) ;
#8501 = CARTESIAN_POINT ( 'NONE',  ( -15.99999999999999289, 79.99999999999998579, -12.50000000000000178 ) ) ;
#8502 = CARTESIAN_POINT ( 'NONE',  ( 221.7323030100353662, 32.17036527648973276, -14.00000000000005507 ) ) ;
#8503 = DIRECTION ( 'NONE',  ( -0.5943026915289565393, -0.3431208189343671333, 0.7273736415730550631 ) ) ;
#8504 = EDGE_CURVE ( 'NONE', #3298, #14420, #15280, .T. ) ;
#8505 = EDGE_LOOP ( 'NONE', ( #2057, #7837, #4515, #16851 ) ) ;
#8506 = CIRCLE ( 'NONE', #7489, 4.999999999999990230 ) ;
#8507 = ADVANCED_FACE ( 'NONE', ( #10087 ), #19750, .T. ) ;
#8508 = B_SPLINE_CURVE_WITH_KNOTS ( 'NONE', 3,
 ( #8985, #4126, #17065, #15488 ),
 .UNSPECIFIED., .F., .F.,
 ( 4, 4 ),
 ( 4.288785295254672358E-06, 0.0005702150075940168880 ),
 .UNSPECIFIED. ) ;
#8509 = LINE ( 'NONE', #1949, #14989 ) ;
#8510 = AXIS2_PLACEMENT_3D ( 'NONE', #19569, #19677, #5046 ) ;
#8511 = AXIS2_PLACEMENT_3D ( 'NONE', #9723, #1797, #19285 ) ;
#8512 = CARTESIAN_POINT ( 'NONE',  ( 59.22717251798539451, 75.87775315904988815, -5.353841392320322079 ) ) ;
#8513 = LINE ( 'NONE', #18166, #8369 ) ;
#8514 = VERTEX_POINT ( 'NONE', #15221 ) ;
#8516 = EDGE_CURVE ( 'NONE', #12613, #3255, #15117, .T. ) ;
#8515 = CARTESIAN_POINT ( 'NONE',  ( 219.1503276808599594, 36.64940697350503029, -10.80501622924627902 ) ) ;
#8517 = DIRECTION ( 'NONE',  ( 0.4758887346169486388, 0.2747544890354095548, 0.8354878114129317135 ) ) ;
#8518 = CARTESIAN_POINT ( 'NONE',  ( 206.7681187495013262, 14.79532522365839675, -2.669358488461178069 ) ) ;
#8519 = CARTESIAN_POINT ( 'NONE',  ( -7.416086753897887185, 79.99999999992817834, -9.098350519373953560 ) ) ;
#8521 = ORIENTED_EDGE ( 'NONE', *, *, #9384, .T. ) ;
#8520 = ORIENTED_EDGE ( 'NONE', *, *, #16319, .T. ) ;
#8522 = DIRECTION ( 'NONE',  ( -0.7235536692358650601, -0.4177439057064745165, -0.5495089780708014571 ) ) ;
#8523 = DIRECTION ( 'NONE',  ( -0.5000000000000051070, 0.8660254037844359321, -0.000000000000000000 ) ) ;
#8524 = DIRECTION ( 'NONE',  ( -0.8660254037844357100, -0.5000000000000051070, 0.000000000000000000 ) ) ;
#8525 = ADVANCED_FACE ( 'NONE', ( #13302 ), #3636, .F. ) ;
#8526 = AXIS2_PLACEMENT_3D ( 'NONE', #147, #14797, #6382 ) ;
#8527 = MECHANICAL_DESIGN_GEOMETRIC_PRESENTATION_REPRESENTATION (  '', ( #9552 ), #13630 ) ;
#8528 = DIRECTION ( 'NONE',  ( -0.7071067811865462405, 0.000000000000000000, 0.7071067811865489050 ) ) ;
#8529 = CARTESIAN_POINT ( 'NONE',  ( -27.42820750412292341, 6.346396126445347008, 5.151021229765904152 ) ) ;
#8530 = SHAPE_REPRESENTATION_RELATIONSHIP ( 'NONE' , 'NONE' ,  #20473, #19205 ) ;
#8531 = CARTESIAN_POINT ( 'NONE',  ( 37.00490953756720813, 229.8619860023653132, 26.00000000000001776 ) ) ;
#8532 = EDGE_LOOP ( 'NONE', ( #16918, #13121, #18521, #20889, #8165, #6117, #5147, #18912 ) ) ;
#8533 = CARTESIAN_POINT ( 'NONE',  ( 82.11984465641647546, 64.23705030780924119, -25.48156911047034612 ) ) ;
#8534 = CARTESIAN_POINT ( 'NONE',  ( -5.556399631426875985, 45.18150654375704534, -6.911722607583233646 ) ) ;
#8535 = VERTEX_POINT ( 'NONE', #3851 ) ;
#8536 = CARTESIAN_POINT ( 'NONE',  ( 202.5825078627354117, 24.78475806348888000, -15.45148755736461510 ) ) ;
#8537 = CARTESIAN_POINT ( 'NONE',  ( -3.526256370528186412, 48.49133988427076503, -0.8569032390966567769 ) ) ;
#8538 = CARTESIAN_POINT ( 'NONE',  ( -2.443633760204237504, 79.40511245435270382, -8.308716123878882698 ) ) ;
#8539 = AXIS2_PLACEMENT_3D ( 'NONE', #16887, #5530, #12018 ) ;
#8540 = VECTOR ( 'NONE', #10722, 1000.000000000000227 ) ;
#8541 = CARTESIAN_POINT ( 'NONE',  ( 229.4064455670339555, 36.39231742674856918, -12.92165662794199577 ) ) ;
#8542 = CARTESIAN_POINT ( 'NONE',  ( 208.8107687779841228, 4.427644383670616079, -14.00000000000005507 ) ) ;
#8543 = AXIS2_PLACEMENT_3D ( 'NONE', #18414, #4309, #4520 ) ;
#8544 = CARTESIAN_POINT ( 'NONE',  ( 197.3251902926419348, 19.95812166752348205, -1.717498466822807490 ) ) ;
#8546 = ORIENTED_EDGE ( 'NONE', *, *, #1901, .T. ) ;
#8545 = ORIENTED_EDGE ( 'NONE', *, *, #17851, .F. ) ;
#8547 = VERTEX_POINT ( 'NONE', #2060 ) ;
#8548 = CARTESIAN_POINT ( 'NONE',  ( 199.6965843892926671, 23.56992829431497327, -14.00000000000005507 ) ) ;
#8549 = CARTESIAN_POINT ( 'NONE',  ( 218.5578050973448683, 38.29353456212945872, -11.94979443502191074 ) ) ;
#8550 = ORIENTED_EDGE ( 'NONE', *, *, #8594, .F. ) ;
#8551 = DIRECTION ( 'NONE',  ( -0.8660254037844360431, -0.5000000000000043299, 0.000000000000000000 ) ) ;
#8552 = PRODUCT ( 'socket head cap screw_iso_ISO 4762 M10 x 16 - 16N', 'socket head cap screw_iso_ISO 4762 M10 x 16 - 16N', '', ( #1188 ) ) ;
#8553 = CARTESIAN_POINT ( 'NONE',  ( 217.3836630237427983, 9.377207184193595779, -7.515250618841534447 ) ) ;
#8554 = LINE ( 'NONE', #8659, #11047 ) ;
#8555 = VERTEX_POINT ( 'NONE', #474 ) ;
#8556 = CARTESIAN_POINT ( 'NONE',  ( 215.2334520059837359, 15.55878974066576070, -9.972943347742017295 ) ) ;
#8557 = CARTESIAN_POINT ( 'NONE',  ( 64.99529059433392320, 211.3812238888322952, 6.000000000000009770 ) ) ;
#8558 = AXIS2_PLACEMENT_3D ( 'NONE', #1484, #17708, #7929 ) ;
#8559 = ORIENTED_EDGE ( 'NONE', *, *, #9400, .T. ) ;
#8560 = ADVANCED_FACE ( 'NONE', ( #674 ), #6816, .T. ) ;
#8561 = DIRECTION ( 'NONE',  ( 0.000000000000000000, 1.000000000000000000, 0.000000000000000000 ) ) ;
#8562 = DIRECTION ( 'NONE',  ( -0.000000000000000000, -1.000000000000000000, -0.000000000000000000 ) ) ;
#8563 = CARTESIAN_POINT ( 'NONE',  ( -33.41199867414998437, 54.49694147696414603, -1.784705491317941206 ) ) ;
#8564 = CARTESIAN_POINT ( 'NONE',  ( 206.4411508673863409, 9.951503049707822512, -1.545471579934816875 ) ) ;
#8565 = CARTESIAN_POINT ( 'NONE',  ( 208.0983737146324870, 5.661548828456886895, -14.00000000000005507 ) ) ;
#8566 = CARTESIAN_POINT ( 'NONE',  ( 9.999999999999998224, -3.747002708109903570E-17, -5.400000000000040323 ) ) ;
#8567 = EDGE_CURVE ( 'NONE', #10275, #14507, #370, .T. ) ;
#8569 = ORIENTED_EDGE ( 'NONE', *, *, #16067, .F. ) ;
#8568 = ORIENTED_EDGE ( 'NONE', *, *, #8994, .T. ) ;
#8570 = ORIENTED_EDGE ( 'NONE', *, *, #18469, .F. ) ;
#8571 = VECTOR ( 'NONE', #16350, 1000.000000000000227 ) ;
#8572 = CARTESIAN_POINT ( 'NONE',  ( 62.17916131348992081, 78.42313103979506650, -13.88866078518543112 ) ) ;
#8573 = EDGE_LOOP ( 'NONE', ( #3620, #8058, #20714, #8197, #5686, #12069 ) ) ;
#8574 = ORIENTED_EDGE ( 'NONE', *, *, #16264, .F. ) ;
#8575 = CARTESIAN_POINT ( 'NONE',  ( 159.9952905943347901, 46.83639716978954226, -6.000000000000052403 ) ) ;
#8576 = DIRECTION ( 'NONE',  ( -0.5000000000000054401, 0.8660254037844354880, -0.000000000000000000 ) ) ;
#8577 = EDGE_LOOP ( 'NONE', ( #10233, #8139, #15953, #10422 ) ) ;
#8578 = DIRECTION ( 'NONE',  ( 0.5000000000000051070, -0.8660254037844358210, 0.000000000000000000 ) ) ;
#8579 = ORIENTED_EDGE ( 'NONE', *, *, #18171, .F. ) ;
#8580 = EDGE_CURVE ( 'NONE', #12707, #19959, #2168, .T. ) ;
#8581 = FACE_OUTER_BOUND ( 'NONE', #12239, .T. ) ;
#8582 = VERTEX_POINT ( 'NONE', #5318 ) ;
#8583 = VECTOR ( 'NONE', #5836, 1000.000000000000000 ) ;
#8584 = DIRECTION ( 'NONE',  ( -0.5000000000000008882, 0.8660254037844381525, 0.000000000000000000 ) ) ;
#8585 = AXIS2_PLACEMENT_3D ( 'NONE', #18564, #4461, #17182 ) ;
#8586 = DIRECTION ( 'NONE',  ( 0.8660254037844355990, 0.5000000000000054401, 8.343535232742331521E-16 ) ) ;
#8587 = CARTESIAN_POINT ( 'NONE',  ( 228.5397721961435593, 38.87290562976085795, -17.42570676230502968 ) ) ;
#8588 = DIRECTION ( 'NONE',  ( 0.4895420438411626773, -0.8479116923739991041, 0.2034560130526446298 ) ) ;
#8589 = DIRECTION ( 'NONE',  ( -0.2961981327260172492, -0.1710100716628330242, 0.9396926207859107594 ) ) ;
#8590 = EDGE_CURVE ( 'NONE', #13223, #18465, #18287, .T. ) ;
#8591 = CARTESIAN_POINT ( 'NONE',  ( 61.99529059433388767, 216.5773763115390693, 1.000000000000017097 ) ) ;
#8592 = LINE ( 'NONE', #16865, #6540 ) ;
#8593 = CARTESIAN_POINT ( 'NONE',  ( 221.6105054788284292, 32.80012433514488635, -11.63296046036689901 ) ) ;
#8594 = EDGE_CURVE ( 'NONE', #15541, #11249, #572, .T. ) ;
#8595 = ORIENTED_EDGE ( 'NONE', *, *, #5381, .T. ) ;
#8596 = CARTESIAN_POINT ( 'NONE',  ( -2.018562491348669496, 65.74999999999998579, 2.826871295670243978 ) ) ;
#8597 = CARTESIAN_POINT ( 'NONE',  ( -15.28360237041720282, 71.55916543031763410, -4.951609446663259639 ) ) ;
#8598 = CARTESIAN_POINT ( 'NONE',  ( 75.23666811385876940, 52.27308886237457841, -15.20134910407188400 ) ) ;
#8600 = EDGE_LOOP ( 'NONE', ( #2424, #3212, #17838, #4076 ) ) ;
#8599 = ORIENTED_EDGE ( 'NONE', *, *, #9260, .F. ) ;
#8601 = ADVANCED_FACE ( 'NONE', ( #13509 ), #17965, .T. ) ;
#8602 = EDGE_LOOP ( 'NONE', ( #18865, #19274, #18155, #9062 ) ) ;
#8603 = CARTESIAN_POINT ( 'NONE',  ( 212.8872982515398178, 6.781229772587438198, -24.85758746085098991 ) ) ;
#8604 = ORIENTED_EDGE ( 'NONE', *, *, #9485, .T. ) ;
#8605 = CARTESIAN_POINT ( 'NONE',  ( 76.47376643088200865, 53.92683595214138137, -5.681768602789493805 ) ) ;
#8606 = B_SPLINE_CURVE_WITH_KNOTS ( 'NONE', 3,
 ( #4085, #10539, #12260, #20912 ),
 .UNSPECIFIED., .F., .F.,
 ( 4, 4 ),
 ( 2.252543412771517539E-07, 0.0005857136100808965759 ),
 .UNSPECIFIED. ) ;
#8607 = CARTESIAN_POINT ( 'NONE',  ( 211.7854512130869580, 13.56808555472074751, -4.379064819896290928 ) ) ;
#8608 = CARTESIAN_POINT ( 'NONE',  ( 219.2728015091131510, 36.40725127431072394, -17.30537846547894176 ) ) ;
#8609 = CARTESIAN_POINT ( 'NONE',  ( 220.8683653123198667, 33.87959670730602824, -10.71100983847133037 ) ) ;
#8610 = EDGE_CURVE ( 'NONE', #206, #17110, #7237, .T. ) ;
#8611 = ORIENTED_EDGE ( 'NONE', *, *, #11304, .T. ) ;
#8612 = CARTESIAN_POINT ( 'NONE',  ( 30.00000000000000000, -9.999999999999998224, 15.00000000000000000 ) ) ;
#8613 = CIRCLE ( 'NONE', #11331, 4.999999999999968026 ) ;
#8614 = EDGE_CURVE ( 'NONE', #20919, #1328, #19955, .T. ) ;
#8615 = DIRECTION ( 'NONE',  ( 0.5000000000000046629, -0.8660254037844360431, -4.006172263299081054E-16 ) ) ;
#8616 = CARTESIAN_POINT ( 'NONE',  ( -31.34819869032959261, 64.25000000000002842, 2.481238266578627893 ) ) ;
#8617 = ORIENTED_EDGE ( 'NONE', *, *, #9622, .F. ) ;
#8618 = SURFACE_STYLE_USAGE ( .BOTH. , #5215 ) ;
#8619 = CARTESIAN_POINT ( 'NONE',  ( 206.6806582365933593, 10.62083195558481741, -15.36420995827523228 ) ) ;
#8620 = CARTESIAN_POINT ( 'NONE',  ( 28.00000000000001066, 65.00000000000000000, -12.50000000000000000 ) ) ;
#8621 = CARTESIAN_POINT ( 'NONE',  ( -4.530168698509680070, 79.99999999986593480, -4.984538917061887453 ) ) ;
#8622 = EDGE_CURVE ( 'NONE', #16061, #15437, #4050, .T. ) ;
#8624 = ORIENTED_EDGE ( 'NONE', *, *, #1780, .T. ) ;
#8623 = ORIENTED_EDGE ( 'NONE', *, *, #4924, .F. ) ;
#8625 = ORIENTED_EDGE ( 'NONE', *, *, #20750, .T. ) ;
#8626 = EDGE_CURVE ( 'NONE', #166, #4564, #11920, .T. ) ;
#8627 = CARTESIAN_POINT ( 'NONE',  ( -14.99999999999999822, -10.00000000000000000, -28.99999999999999645 ) ) ;
#8628 = DIRECTION ( 'NONE',  ( 0.8660254037844380415, 0.5000000000000014433, 0.000000000000000000 ) ) ;
#8629 = DIRECTION ( 'NONE',  ( -0.8660254037844355990, -0.5000000000000054401, 0.000000000000000000 ) ) ;
#8630 = CARTESIAN_POINT ( 'NONE',  ( 81.85908840240438167, 56.78121513735760573, -23.59847208966338528 ) ) ;
#8631 = AXIS2_PLACEMENT_3D ( 'NONE', #8818, #10822, #17199 ) ;
#8632 = CARTESIAN_POINT ( 'NONE',  ( -26.39566432206697755, 9.975777012415697698, 6.949400359526464399 ) ) ;
#8633 = FACE_OUTER_BOUND ( 'NONE', #2272, .T. ) ;
#8634 = EDGE_CURVE ( 'NONE', #4202, #19075, #7336, .T. ) ;
#8635 = EDGE_LOOP ( 'NONE', ( #8482, #5461, #1600, #1660 ) ) ;
#8636 = CARTESIAN_POINT ( 'NONE',  ( 81.59473887788738011, 64.10409879185415605, -25.47155011481813602 ) ) ;
#8637 = CARTESIAN_POINT ( 'NONE',  ( 215.6183575532814416, 34.49441912408899924, -14.00000000000004441 ) ) ;
#8638 = ORIENTED_EDGE ( 'NONE', *, *, #12117, .T. ) ;
#8639 = CARTESIAN_POINT ( 'NONE',  ( 201.9232846251233013, 26.15919357289564218, -14.99235525741147868 ) ) ;
#8640 = CARTESIAN_POINT ( 'NONE',  ( -3.276752736765743634, 61.69737001983726543, 2.155802286817233959 ) ) ;
#8641 = CARTESIAN_POINT ( 'NONE',  ( 1.486836232935293767, 76.55853692374149944, -2.936780385859808717 ) ) ;
#8642 = EDGE_CURVE ( 'NONE', #13417, #18641, #8813, .T. ) ;
#8643 = CARTESIAN_POINT ( 'NONE',  ( 43.00000000000000000, 4.475777889183787821E-16, -3.309499999999999886 ) ) ;
#8644 = CARTESIAN_POINT ( 'NONE',  ( 98.77077497239712045, 200.0086332439910279, 8.500000000000021316 ) ) ;
#8645 = CARTESIAN_POINT ( 'NONE',  ( -31.74999999999995737, 7.960204194457795477E-16, -6.500000000000000000 ) ) ;
#8646 = AXIS2_PLACEMENT_3D ( 'NONE', #18032, #15297, #7401 ) ;
#8648 = ORIENTED_EDGE ( 'NONE', *, *, #16667, .F. ) ;
#8647 = ORIENTED_EDGE ( 'NONE', *, *, #19344, .F. ) ;
#8649 = ORIENTED_EDGE ( 'NONE', *, *, #4924, .T. ) ;
#8650 = AXIS2_PLACEMENT_3D ( 'NONE', #12090, #3504, #5500 ) ;
#8651 = ORIENTED_EDGE ( 'NONE', *, *, #6238, .F. ) ;
#8652 = LINE ( 'NONE', #2514, #10515 ) ;
#8653 = LINE ( 'NONE', #13540, #5780 ) ;
#8654 = B_SPLINE_CURVE_WITH_KNOTS ( 'NONE', 3,
 ( #1627, #8181, #143, #16162, #14579, #40, #6479, #11478, #3116, #17853, #19426, #14687, #11066, #6582 ),
 .UNSPECIFIED., .F., .F.,
 ( 4, 2, 2, 2, 2, 2, 4 ),
 ( 0.000000000000000000, 0.001520696258467074333, 0.003041392516934148665, 0.006082785033868297331, 0.007603481292335390745, 0.009124177550802484160, 0.01216557006773670568 ),
 .UNSPECIFIED. ) ;
#8655 = ORIENTED_EDGE ( 'NONE', *, *, #11982, .F. ) ;
#8656 = VERTEX_POINT ( 'NONE', #19119 ) ;
#8657 = CARTESIAN_POINT ( 'NONE',  ( 42.39721438298049350, 244.5222400402098231, -13.99999999999997513 ) ) ;
#8658 = CARTESIAN_POINT ( 'NONE',  ( 218.2448338841374493, 36.70426184694303373, -11.10922658182122724 ) ) ;
#8659 = CARTESIAN_POINT ( 'NONE',  ( -31.74999999999995737, 3.469446951953614189E-17, 5.000000000000036415 ) ) ;
#8660 =( REPRESENTATION_RELATIONSHIP ('NONE','NONE', #4634, #14136 ) REPRESENTATION_RELATIONSHIP_WITH_TRANSFORMATION ( #20673 )SHAPE_REPRESENTATION_RELATIONSHIP( ) );
#8661 = VERTEX_POINT ( 'NONE', #20272 ) ;
#8662 = FACE_OUTER_BOUND ( 'NONE', #16499, .T. ) ;
#8663 = CARTESIAN_POINT ( 'NONE',  ( -19.99144900083270215, 68.18358604705119319, -3.013858250467852606 ) ) ;
#8664 = CIRCLE ( 'NONE', #3922, 12.47473710546057823 ) ;
#8665 = ORIENTED_EDGE ( 'NONE', *, *, #7983, .F. ) ;
#8666 = VECTOR ( 'NONE', #18023, 1000.000000000000227 ) ;
#8667 = AXIS2_PLACEMENT_3D ( 'NONE', #2216, #8778, #15275 ) ;
#8668 = CARTESIAN_POINT ( 'NONE',  ( 199.2144802262915846, 21.04890371929339921, -14.00000000000005507 ) ) ;
#8669 = LINE ( 'NONE', #18425, #11595 ) ;
#8670 = CARTESIAN_POINT ( 'NONE',  ( -28.62507391571850945, 53.64368112681762568, -2.695303598069996642 ) ) ;
#8671 = DIRECTION ( 'NONE',  ( -1.000000000000000000, 0.000000000000000000, 0.000000000000000000 ) ) ;
#8672 = DIRECTION ( 'NONE',  ( 0.8660254037844371533, 0.5000000000000027756, -0.000000000000000000 ) ) ;
#8673 = DIRECTION ( 'NONE',  ( 0.000000000000000000, 1.000000000000000000, -1.224646799147353207E-16 ) ) ;
#8675 = ORIENTED_EDGE ( 'NONE', *, *, #7247, .F. ) ;
#8674 = ORIENTED_EDGE ( 'NONE', *, *, #6308, .F. ) ;
#8676 = VECTOR ( 'NONE', #12872, 1000.000000000000114 ) ;
#8677 = CARTESIAN_POINT ( 'NONE',  ( 54.37566476943453608, 77.94482555308654526, -13.72387178829551502 ) ) ;
#8678 = VECTOR ( 'NONE', #10873, 1000.000000000000000 ) ;
#8679 = ORIENTED_EDGE ( 'NONE', *, *, #20264, .T. ) ;
#8680 = CARTESIAN_POINT ( 'NONE',  ( 220.2180084519553134, 35.41797800104779270, -14.00000000000005507 ) ) ;
#8681 = VECTOR ( 'NONE', #11694, 1000.000000000000114 ) ;
#8682 = DIRECTION ( 'NONE',  ( -0.8660254037844355990, -0.5000000000000051070, -2.294936594593527877E-16 ) ) ;
#8683 = VERTEX_POINT ( 'NONE', #17420 ) ;
#8684 = DIRECTION ( 'NONE',  ( 0.000000000000000000, 0.000000000000000000, -1.000000000000000000 ) ) ;
#8685 = CARTESIAN_POINT ( 'NONE',  ( 219.5521249847671186, 36.57132199813789697, -10.33191597617938484 ) ) ;
#8686 = ORIENTED_EDGE ( 'NONE', *, *, #14345, .F. ) ;
#8687 = ADVANCED_FACE ( 'NONE', ( #4591 ), #19016, .T. ) ;
#8688 = CARTESIAN_POINT ( 'NONE',  ( 32.36389338619004263, 157.9004617752989930, -12.50000000000000000 ) ) ;
#8689 = DIRECTION ( 'NONE',  ( 0.8660254037844361541, 0.5000000000000043299, -5.976026924694053325E-17 ) ) ;
#8690 = AXIS2_PLACEMENT_3D ( 'NONE', #19494, #532, #11665 ) ;
#8691 = DIRECTION ( 'NONE',  ( 0.03124427847888232648, 0.6611148994991496997, -0.7496338337632335591 ) ) ;
#8692 = CARTESIAN_POINT ( 'NONE',  ( 198.5772061109008746, 5.942301689450959046, -22.62267072728657169 ) ) ;
#8693 = CARTESIAN_POINT ( 'NONE',  ( 30.10683012259193703, 0.000000000000000000, -5.999999999999998224 ) ) ;
#8694 = ORIENTED_EDGE ( 'NONE', *, *, #17561, .F. ) ;
#8695 = CARTESIAN_POINT ( 'NONE',  ( -33.31284561364699215, 74.81579058300519591, -1.112382790401626798 ) ) ;
#8696 = CARTESIAN_POINT ( 'NONE',  ( 0.000000000000000000, -1.759474945355379072, 3.047500000000001652 ) ) ;
#8697 = CARTESIAN_POINT ( 'NONE',  ( 204.9818247258934321, 9.640009970873835599, -2.187257959407756136 ) ) ;
#8698 = ORIENTED_EDGE ( 'NONE', *, *, #4826, .T. ) ;
#8699 = CARTESIAN_POINT ( 'NONE',  ( 81.85522543128666939, 56.76562253233274902, -1.406549998271479751 ) ) ;
#8700 = EDGE_CURVE ( 'NONE', #15178, #20230, #20481, .T. ) ;
#8701 = ORIENTED_EDGE ( 'NONE', *, *, #6886, .T. ) ;
#8702 = CARTESIAN_POINT ( 'NONE',  ( 194.1867014016589508, 7.531440531094472313, -18.06789442459577444 ) ) ;
#8703 = CARTESIAN_POINT ( 'NONE',  ( 220.1214136286681651, 10.95784823292136956, -12.41782726985285379 ) ) ;
#8704 = ORIENTED_EDGE ( 'NONE', *, *, #20892, .T. ) ;
#8705 = VECTOR ( 'NONE', #9719, 1000.000000000000227 ) ;
#8706 = DIRECTION ( 'NONE',  ( 1.000000000000000000, 0.000000000000000000, 0.000000000000000000 ) ) ;
#8707 = EDGE_CURVE ( 'NONE', #15290, #10440, #4276, .T. ) ;
#8708 = DIRECTION ( 'NONE',  ( 0.000000000000000000, 0.000000000000000000, 1.000000000000000000 ) ) ;
#8709 = ORIENTED_EDGE ( 'NONE', *, *, #19087, .T. ) ;
#8710 = CARTESIAN_POINT ( 'NONE',  ( 81.52759066145694078, 64.25397585761884045, -25.47962019146266499 ) ) ;
#8711 = EDGE_CURVE ( 'NONE', #5234, #16498, #10834, .T. ) ;
#8712 = CARTESIAN_POINT ( 'NONE',  ( 218.8737197432240293, 10.23749183229395676, -11.23040475586419085 ) ) ;
#8713 = LINE ( 'NONE', #15211, #562 ) ;
#8714 = CARTESIAN_POINT ( 'NONE',  ( 229.5841978618468033, 37.06390731203416777, -15.46846178913027714 ) ) ;
#8715 = ORIENTED_EDGE ( 'NONE', *, *, #14358, .T. ) ;
#8716 = CARTESIAN_POINT ( 'NONE',  ( 207.9638137018049804, 4.453860881324136045, -26.27710986211782895 ) ) ;
#8717 = CARTESIAN_POINT ( 'NONE',  ( 226.9422368340881064, 41.31344896776308673, -17.27917287590617335 ) ) ;
#8718 = AXIS2_PLACEMENT_3D ( 'NONE', #6069, #17117, #12565 ) ;
#8719 = CARTESIAN_POINT ( 'NONE',  ( 220.2040058117674164, 11.00553285206667908, -14.05525385477321443 ) ) ;
#8720 = ORIENTED_EDGE ( 'NONE', *, *, #10687, .T. ) ;
#8721 = CARTESIAN_POINT ( 'NONE',  ( 217.3439437943931409, 38.26464925441550236, -12.30768923015392780 ) ) ;
#8723 = DIRECTION ( 'NONE',  ( -0.8660254037844362651, -0.5000000000000045519, 5.976026924694053325E-17 ) ) ;
#8722 = VECTOR ( 'NONE', #9201, 1000.000000000000000 ) ;
#8724 = PRODUCT_DEFINITION ( 'UNKNOWN', '', #5024, #16159 ) ;
#8725 = DIRECTION ( 'NONE',  ( 1.000000000000000000, 0.000000000000000000, 0.000000000000000000 ) ) ;
#8726 = CARTESIAN_POINT ( 'NONE',  ( 220.7476224395899465, 32.36930490829749374, -17.10689588174070153 ) ) ;
#8727 = EDGE_CURVE ( 'NONE', #16824, #12098, #18632, .T. ) ;
#8728 = ORIENTED_EDGE ( 'NONE', *, *, #13128, .T. ) ;
#8729 = EDGE_LOOP ( 'NONE', ( #8148, #4153, #18230, #7110, #12265 ) ) ;
#8730 = ORIENTED_EDGE ( 'NONE', *, *, #12948, .T. ) ;
#8731 = DIRECTION ( 'NONE',  ( 0.8660254037844362651, 0.5000000000000039968, -0.000000000000000000 ) ) ;
#8732 = DIRECTION ( 'NONE',  ( 0.5000000000000038858, -0.8660254037844362651, 0.000000000000000000 ) ) ;
#8733 = CARTESIAN_POINT ( 'NONE',  ( -33.49470602546865905, 76.40689540430931004, -2.756335249929798614 ) ) ;
#8734 = EDGE_CURVE ( 'NONE', #19670, #2016, #4380, .T. ) ;
#8735 = CARTESIAN_POINT ( 'NONE',  ( 80.72516319149150377, 53.31353001781401701, -21.13911636830589558 ) ) ;
#8736 = AXIS2_PLACEMENT_3D ( 'NONE', #11889, #7408, #7211 ) ;
#8737 = CARTESIAN_POINT ( 'NONE',  ( 212.5692528822464737, 18.14461157680397108, -5.585956497640101048 ) ) ;
#8738 = EDGE_CURVE ( 'NONE', #255, #13116, #18996, .T. ) ;
#8739 = ORIENTED_EDGE ( 'NONE', *, *, #9528, .F. ) ;
#8740 = CARTESIAN_POINT ( 'NONE',  ( 82.12886169804700387, 61.33916772676509055, -24.97880947958990561 ) ) ;
#8741 = ADVANCED_FACE ( 'NONE', ( #1203 ), #17209, .F. ) ;
#8742 = CARTESIAN_POINT ( 'NONE',  ( 60.52928988819383704, 83.99806976322641106, -17.46522718495289439 ) ) ;
#8743 = EDGE_CURVE ( 'NONE', #12993, #1364, #7655, .T. ) ;
#8744 = CARTESIAN_POINT ( 'NONE',  ( 203.2929909647774593, 23.96012768562937367, -14.39487826001324500 ) ) ;
#8745 = CARTESIAN_POINT ( 'NONE',  ( 192.0123155716599683, 35.38128320186102371, -18.91295074164679235 ) ) ;
#8746 = CARTESIAN_POINT ( 'NONE',  ( 98.91428619100412334, 200.0914894846854679, 13.49999999999996803 ) ) ;
#8747 = FACE_OUTER_BOUND ( 'NONE', #13177, .T. ) ;
#8748 = CARTESIAN_POINT ( 'NONE',  ( 30.00000000000000355, 5.000000000000000000, -15.00000000000000000 ) ) ;
#8749 = LINE ( 'NONE', #15355, #5226 ) ;
#8751 = ORIENTED_EDGE ( 'NONE', *, *, #3208, .F. ) ;
#8750 = EDGE_LOOP ( 'NONE', ( #13434, #16602, #8570 ) ) ;
#8752 = ORIENTED_EDGE ( 'NONE', *, *, #12097, .F. ) ;
#8753 = VERTEX_POINT ( 'NONE', #8933 ) ;
#8754 = LINE ( 'NONE', #506, #3413 ) ;
#8755 = CARTESIAN_POINT ( 'NONE',  ( 229.0363929556513369, 37.03326735113697055, -16.48323849494068227 ) ) ;
#8756 = EDGE_CURVE ( 'NONE', #1288, #8514, #20232, .T. ) ;
#8757 = VERTEX_POINT ( 'NONE', #9298 ) ;
#8758 = EDGE_LOOP ( 'NONE', ( #19563, #14565, #13610, #20431 ) ) ;
#8759 = EDGE_LOOP ( 'NONE', ( #16441, #8675, #6464, #19884, #17478 ) ) ;
#8760 = EDGE_LOOP ( 'NONE', ( #7704, #14983, #18051, #5070, #14259 ) ) ;
#8761 = DIRECTION ( 'NONE',  ( 0.000000000000000000, -0.5000000000000008882, -0.8660254037844380415 ) ) ;
#8762 = DIRECTION ( 'NONE',  ( -1.000000000000000000, 0.000000000000000000, 0.000000000000000000 ) ) ;
#8763 = PLANE ( 'NONE',  #16142 ) ;
#8764 = ORIENTED_EDGE ( 'NONE', *, *, #7026, .T. ) ;
#8765 = LINE ( 'NONE', #7171, #7956 ) ;
#8766 = CARTESIAN_POINT ( 'NONE',  ( -20.13425257954909142, 67.51366979390380152, -2.814775708409672728 ) ) ;
#8767 = EDGE_CURVE ( 'NONE', #330, #3291, #13933, .T. ) ;
#8768 = EDGE_CURVE ( 'NONE', #17870, #14892, #18477, .T. ) ;
#8769 = ORIENTED_EDGE ( 'NONE', *, *, #7124, .T. ) ;
#8770 = VECTOR ( 'NONE', #16210, 1000.000000000000227 ) ;
#8771 = CARTESIAN_POINT ( 'NONE',  ( 205.1351227324282718, 9.374490034856508558, -1.709088388254546453 ) ) ;
#8772 = EDGE_CURVE ( 'NONE', #9311, #16889, #12658, .T. ) ;
#8773 = LINE ( 'NONE', #5263, #17682 ) ;
#8774 = CARTESIAN_POINT ( 'NONE',  ( -28.77462657304674565, 54.25663578079195304, -2.022313059153934223 ) ) ;
#8775 = CYLINDRICAL_SURFACE ( 'NONE', #6189, 8.000000000000058620 ) ;
#8776 = CARTESIAN_POINT ( 'NONE',  ( 228.6663896750565357, 38.65359772315768794, -18.00871210835857639 ) ) ;
#8777 = EDGE_CURVE ( 'NONE', #17576, #15613, #6110, .T. ) ;
#8778 = DIRECTION ( 'NONE',  ( -0.4330127018922209636, -0.2500000000000048850, -0.8660254037844363761 ) ) ;
#8780 = ORIENTED_EDGE ( 'NONE', *, *, #1227, .F. ) ;
#8779 = VERTEX_POINT ( 'NONE', #1619 ) ;
#8781 = CARTESIAN_POINT ( 'NONE',  ( 62.17277006171050147, 78.42718308225904877, -13.70364326203602268 ) ) ;
#8782 = EDGE_CURVE ( 'NONE', #6779, #20850, #5812, .T. ) ;
#8783 = EDGE_LOOP ( 'NONE', ( #2433, #19629 ) ) ;
#8784 = CONICAL_SURFACE ( 'NONE', #6064, 10.85470691220533190, 0.8171114040043576665 ) ;
#8785 = ORIENTED_EDGE ( 'NONE', *, *, #9384, .F. ) ;
#8786 = DIRECTION ( 'NONE',  ( 0.000000000000000000, -1.000000000000000000, 0.000000000000000000 ) ) ;
#8787 = CARTESIAN_POINT ( 'NONE',  ( 217.4886294373914382, 9.953015810246625961, -20.75355104716125609 ) ) ;
#8788 = ORIENTED_EDGE ( 'NONE', *, *, #6672, .T. ) ;
#8789 = EDGE_LOOP ( 'NONE', ( #13994, #9032, #15031, #8433, #11341 ) ) ;
#8790 = CARTESIAN_POINT ( 'NONE',  ( 0.000000000000000000, 0.000000000000000000, 0.000000000000000000 ) ) ;
#8791 = ORIENTED_EDGE ( 'NONE', *, *, #20750, .F. ) ;
#8792 = EDGE_CURVE ( 'NONE', #20070, #3073, #8170, .T. ) ;
#8793 = CIRCLE ( 'NONE', #11171, 2.499999999999994671 ) ;
#8794 = CARTESIAN_POINT ( 'NONE',  ( 221.0990782203562048, 33.24404722175929550, -16.70098974528093905 ) ) ;
#8795 = DIRECTION ( 'NONE',  ( 0.5000000000000026645, -0.8660254037844370423, 0.000000000000000000 ) ) ;
#8796 = B_SPLINE_CURVE_WITH_KNOTS ( 'NONE', 3,
 ( #7859, #1408, #24, #4889 ),
 .UNSPECIFIED., .F., .F.,
 ( 4, 4 ),
 ( 0.0001045099009071127032, 0.0007771606929556430007 ),
 .UNSPECIFIED. ) ;
#8797 = DIRECTION ( 'NONE',  ( 0.5000000000000052180, -0.8660254037844355990, 1.665334536937734318E-16 ) ) ;
#8798 = CARTESIAN_POINT ( 'NONE',  ( 228.4172419990784704, 38.75866508057305992, -17.51243207492525755 ) ) ;
#8799 = CARTESIAN_POINT ( 'NONE',  ( 226.6211368133091923, 39.11482588413117867, -14.00000000000005507 ) ) ;
#8800 = CARTESIAN_POINT ( 'NONE',  ( 1.500000000000001332, 0.000000000000000000, 0.000000000000000000 ) ) ;
#8801 = CIRCLE ( 'NONE', #6077, 5.000000000000000888 ) ;
#8802 = VERTEX_POINT ( 'NONE', #3205 ) ;
#8803 = CARTESIAN_POINT ( 'NONE',  ( -28.36631829605002508, 78.08772077735660844, 1.916778294987758313 ) ) ;
#8804 = AXIS2_PLACEMENT_3D ( 'NONE', #16194, #16094, #8105 ) ;
#8805 = LINE ( 'NONE', #16659, #19421 ) ;
#8806 = CARTESIAN_POINT ( 'NONE',  ( 159.9952905943347901, 46.83639716978955647, -22.00000000000007816 ) ) ;
#8807 = VERTEX_POINT ( 'NONE', #9661 ) ;
#8808 = CARTESIAN_POINT ( 'NONE',  ( -4.498192030073390413, 65.74999999999998579, 4.917728941844615953 ) ) ;
#8809 = EDGE_CURVE ( 'NONE', #20124, #7899, #18250, .T. ) ;
#8810 = ORIENTED_EDGE ( 'NONE', *, *, #13180, .T. ) ;
#8811 = LINE ( 'NONE', #19934, #15923 ) ;
#8812 = DIRECTION ( 'NONE',  ( 1.000000000000000000, 1.110223024625156540E-15, 0.000000000000000000 ) ) ;
#8813 = CIRCLE ( 'NONE', #11529, 4.999999999999968026 ) ;
#8814 = DIRECTION ( 'NONE',  ( -0.8660254037844360431, -0.5000000000000045519, -4.336808689942050277E-16 ) ) ;
#8815 = EDGE_LOOP ( 'NONE', ( #12323, #16357 ) ) ;
#8816 = CARTESIAN_POINT ( 'NONE',  ( 81.63447678882555181, 62.38330499993598011, -25.23821314459116394 ) ) ;
#8817 = CARTESIAN_POINT ( 'NONE',  ( -24.06039977493734483, 79.94564677075823056, -11.17290160265476828 ) ) ;
#8818 = CARTESIAN_POINT ( 'NONE',  ( -14.99999999999999645, -10.00000000000000000, -15.00000000000000000 ) ) ;
#8819 = CARTESIAN_POINT ( 'NONE',  ( 218.0783914157424590, 10.03590803213535132, -8.555339712720195777 ) ) ;
#8820 = VECTOR ( 'NONE', #7918, 1000.000000000000114 ) ;
#8821 = EDGE_CURVE ( 'NONE', #7353, #10831, #12671, .T. ) ;
#8822 = DIRECTION ( 'NONE',  ( -0.8296432542242747621, -0.4789947561577490021, 0.2868032327110945912 ) ) ;
#8823 = VECTOR ( 'NONE', #1194, 1000.000000000000114 ) ;
#8824 = LINE ( 'NONE', #2263, #6151 ) ;
#8825 = DIRECTION ( 'NONE',  ( -0.8660254037844348218, -0.5000000000000064393, 0.000000000000000000 ) ) ;
#8826 = ORIENTED_EDGE ( 'NONE', *, *, #19765, .F. ) ;
#8827 = CIRCLE ( 'NONE', #5421, 4.999999999999989342 ) ;
#8828 = DIRECTION ( 'NONE',  ( 0.5000000000000054401, -0.8660254037844353769, 2.220446049250312588E-16 ) ) ;
#8829 = DIRECTION ( 'NONE',  ( 0.000000000000000000, -1.000000000000000000, 0.000000000000000000 ) ) ;
#8830 = AXIS2_PLACEMENT_3D ( 'NONE', #1257, #2850, #1463 ) ;
#8831 = EDGE_CURVE ( 'NONE', #5298, #8387, #14444, .T. ) ;
#8832 = DIRECTION ( 'NONE',  ( -0.000000000000000000, 1.000000000000000000, -0.000000000000000000 ) ) ;
#8833 = FACE_OUTER_BOUND ( 'NONE', #14181, .T. ) ;
#8835 = ORIENTED_EDGE ( 'NONE', *, *, #12005, .T. ) ;
#8834 = ORIENTED_EDGE ( 'NONE', *, *, #4362, .T. ) ;
#8836 = CARTESIAN_POINT ( 'NONE',  ( -28.99999999999999289, -10.00000000000000000, 15.00000000000000178 ) ) ;
#8837 = LINE ( 'NONE', #1318, #14656 ) ;
#8838 = CARTESIAN_POINT ( 'NONE',  ( 227.5312376355471145, 39.64027283883993391, -14.00000000000005507 ) ) ;
#8839 = B_SPLINE_CURVE_WITH_KNOTS ( 'NONE', 3,
 ( #11041, #9022, #2468, #2680 ),
 .UNSPECIFIED., .F., .F.,
 ( 4, 4 ),
 ( 3.309335659996554474E-07, 0.0008543166715507651216 ),
 .UNSPECIFIED. ) ;
#8840 = AXIS2_PLACEMENT_3D ( 'NONE', #7788, #19543, #12997 ) ;
#8841 = CARTESIAN_POINT ( 'NONE',  ( 79.36047190431935405, 49.50000000000002842, -12.49999999998710898 ) ) ;
#8842 = VECTOR ( 'NONE', #15645, 1000.000000000000227 ) ;
#8843 = DIRECTION ( 'NONE',  ( -0.8660254037844360431, -0.5000000000000045519, -0.000000000000000000 ) ) ;
#8844 = ORIENTED_EDGE ( 'NONE', *, *, #17003, .F. ) ;
#8845 = VECTOR ( 'NONE', #3335, 1000.000000000000114 ) ;
#8846 = CARTESIAN_POINT ( 'NONE',  ( 82.73391158952136948, 64.01818219908709295, -25.58603017124621815 ) ) ;
#8847 = CARTESIAN_POINT ( 'NONE',  ( 58.88613401674517434, 85.26164830632635017, -14.51790671232051899 ) ) ;
#8848 = VERTEX_POINT ( 'NONE', #2430 ) ;
#8849 = DIRECTION ( 'NONE',  ( 0.8660254037844371533, 0.5000000000000025535, 6.106226635438359986E-16 ) ) ;
#8850 = DIRECTION ( 'NONE',  ( 0.000000000000000000, 0.000000000000000000, -1.000000000000000000 ) ) ;
#8851 = PLANE ( 'NONE',  #11164 ) ;
#8852 = ADVANCED_FACE ( 'NONE', ( #7282 ), #12294, .T. ) ;
#8853 = LINE ( 'NONE', #18512, #13885 ) ;
#8854 = FACE_OUTER_BOUND ( 'NONE', #480, .T. ) ;
#8855 = EDGE_CURVE ( 'NONE', #18950, #10186, #7461, .T. ) ;
#8856 = ORIENTED_EDGE ( 'NONE', *, *, #12513, .F. ) ;
#8857 = VERTEX_POINT ( 'NONE', #3513 ) ;
#8858 = CARTESIAN_POINT ( 'NONE',  ( 28.00000000000001066, 64.25000000000000000, -1.525597966175989972 ) ) ;
#8860 = CARTESIAN_POINT ( 'NONE',  ( -35.00000000000000000, 65.74999999999997158, -1.525597966176003961 ) ) ;
#8859 = VECTOR ( 'NONE', #8962, 1000.000000000000114 ) ;
#8861 = CIRCLE ( 'NONE', #7164, 5.000000000000001776 ) ;
#8862 = EDGE_LOOP ( 'NONE', ( #10658, #11734, #11664, #3961, #7889, #15793 ) ) ;
#8863 = ORIENTED_EDGE ( 'NONE', *, *, #8998, .T. ) ;
#8864 = PLANE ( 'NONE',  #1395 ) ;
#8865 = CARTESIAN_POINT ( 'NONE',  ( 215.9002224801550085, 8.520742387026412956, -22.69908973750352743 ) ) ;
#8866 = ADVANCED_FACE ( 'NONE', ( #18643 ), #13276, .F. ) ;
#8867 = DIRECTION ( 'NONE',  ( 0.5000000000000057732, -0.8660254037844352659, 0.000000000000000000 ) ) ;
#8868 = CARTESIAN_POINT ( 'NONE',  ( -16.88867936483986654, 71.52687714446561529, -4.923512665565291435 ) ) ;
#8869 = ORIENTED_EDGE ( 'NONE', *, *, #10043, .F. ) ;
#8870 = AXIS2_PLACEMENT_3D ( 'NONE', #2615, #12365, #15246 ) ;
#8871 = ADVANCED_FACE ( 'NONE', ( #4120 ), #16556, .T. ) ;
#8872 = DIRECTION ( 'NONE',  ( 0.000000000000000000, -1.000000000000000000, 0.000000000000000000 ) ) ;
#8873 = CONICAL_SURFACE ( 'NONE', #20047, 13.07248899748297433, 0.6693469023067423196 ) ;
#8874 = EDGE_CURVE ( 'NONE', #17245, #6449, #1047, .T. ) ;
#8875 = FACE_OUTER_BOUND ( 'NONE', #2918, .T. ) ;
#8876 = CARTESIAN_POINT ( 'NONE',  ( -29.20450150413485346, 50.01656837298652647, -11.74597530808301649 ) ) ;
#8877 = DIRECTION ( 'NONE',  ( -1.000000000000000000, 0.000000000000000000, 0.000000000000000000 ) ) ;
#8878 = B_SPLINE_CURVE_WITH_KNOTS ( 'NONE', 3,
 ( #8967, #515, #4105, #2311 ),
 .UNSPECIFIED., .F., .F.,
 ( 4, 4 ),
 ( 6.866270341935863685E-05, 0.0009226484414006754300 ),
 .UNSPECIFIED. ) ;
#8879 = EDGE_CURVE ( 'NONE', #9060, #3430, #4207, .T. ) ;
#8880 = DIRECTION ( 'NONE',  ( 0.000000000000000000, -0.000000000000000000, 1.000000000000000000 ) ) ;
#8881 = CARTESIAN_POINT ( 'NONE',  ( -28.46516275735407220, 48.23356369194445392, -1.109776825402767120 ) ) ;
#8883 = ORIENTED_EDGE ( 'NONE', *, *, #7741, .T. ) ;
#8882 = VERTEX_POINT ( 'NONE', #20433 ) ;
#8884 = CARTESIAN_POINT ( 'NONE',  ( 203.2651618589191571, 23.98739702992933687, -13.51485263443600005 ) ) ;
#8885 = CARTESIAN_POINT ( 'NONE',  ( 59.47741263991522942, 75.77081037196482782, -19.82212451566851286 ) ) ;
#8886 = EDGE_LOOP ( 'NONE', ( #15608, #18316, #13262, #7360 ) ) ;
#8887 = ORIENTED_EDGE ( 'NONE', *, *, #5620, .T. ) ;
#8888 = CARTESIAN_POINT ( 'NONE',  ( -15.99999999999999289, 15.09941697557068530, 0.9999999999999991118 ) ) ;
#8889 = CARTESIAN_POINT ( 'NONE',  ( 218.9706616721823025, 10.29346128107372316, -19.95367855226146148 ) ) ;
#8890 = VECTOR ( 'NONE', #20454, 1000.000000000000114 ) ;
#8891 = EDGE_CURVE ( 'NONE', #1523, #19834, #5055, .T. ) ;
#8892 = VECTOR ( 'NONE', #5670, 1000.000000000000227 ) ;
#8893 = EDGE_CURVE ( 'NONE', #20230, #1364, #16000, .T. ) ;
#8894 = EDGE_LOOP ( 'NONE', ( #10301, #16922, #14962, #3883, #2327, #20177 ) ) ;
#8895 = ORIENTED_EDGE ( 'NONE', *, *, #11184, .T. ) ;
#8896 = DIRECTION ( 'NONE',  ( 1.000000000000000000, 0.000000000000000000, 0.000000000000000000 ) ) ;
#8897 = LINE ( 'NONE', #13786, #13490 ) ;
#8898 = CARTESIAN_POINT ( 'NONE',  ( 216.6495311407713871, 8.953355943939367734, -6.376588578941993823 ) ) ;
#8899 = PRODUCT_DEFINITION_SHAPE ( 'NONE', 'NONE',  #10936 ) ;
#8900 = LINE ( 'NONE', #18770, #3689 ) ;
#8901 = EDGE_CURVE ( 'NONE', #1440, #12607, #12216, .T. ) ;
#8902 = CARTESIAN_POINT ( 'NONE',  ( 228.6687290773336656, 38.64954575955422200, -9.992950739179642383 ) ) ;
#8903 = CARTESIAN_POINT ( 'NONE',  ( 213.9706616721822456, 18.95371531891807848, -19.95367855226146503 ) ) ;
#8904 = DIRECTION ( 'NONE',  ( 0.5000000000000057732, -0.8660254037844353769, 0.000000000000000000 ) ) ;
#8905 = AXIS2_PLACEMENT_3D ( 'NONE', #5920, #1071, #17178 ) ;
#8906 = ORIENTED_EDGE ( 'NONE', *, *, #6283, .F. ) ;
#8907 = CARTESIAN_POINT ( 'NONE',  ( 0.000000000000000000, 0.000000000000000000, 0.000000000000000000 ) ) ;
#8908 = DIRECTION ( 'NONE',  ( 0.000000000000000000, -0.9841898184435619035, 0.1771169141330907193 ) ) ;
#8909 = DIRECTION ( 'NONE',  ( -0.8660254037844363761, -0.5000000000000043299, 6.872020471724002955E-17 ) ) ;
#8910 = ORIENTED_EDGE ( 'NONE', *, *, #16314, .T. ) ;
#8911 = EDGE_CURVE ( 'NONE', #2651, #2349, #17687, .T. ) ;
#8912 = CARTESIAN_POINT ( 'NONE',  ( 80.71088083322737816, 60.18095083263530398, -0.4163648238935768187 ) ) ;
#8913 = VERTEX_POINT ( 'NONE', #20532 ) ;
#8914 = CARTESIAN_POINT ( 'NONE',  ( 200.2088966793999987, 0.2341713026616738524, -22.03054070023845767 ) ) ;
#8915 = FACE_OUTER_BOUND ( 'NONE', #16105, .T. ) ;
#8916 = DIRECTION ( 'NONE',  ( 0.000000000000000000, 0.000000000000000000, 1.000000000000000000 ) ) ;
#8917 = AXIS2_PLACEMENT_3D ( 'NONE', #639, #6659, #11453 ) ;
#8918 = AXIS2_PLACEMENT_3D ( 'NONE', #1713, #8163, #8266 ) ;
#8919 = B_SPLINE_CURVE_WITH_KNOTS ( 'NONE', 3,
 ( #10470, #3912, #17170, #11875 ),
 .UNSPECIFIED., .F., .F.,
 ( 4, 4 ),
 ( 9.556227013665790057E-07, 0.0006736064147440891034 ),
 .UNSPECIFIED. ) ;
#8920 = CARTESIAN_POINT ( 'NONE',  ( 213.3033847652179134, 18.56846281705820090, -6.724618537539641672 ) ) ;
#8921 = ORIENTED_EDGE ( 'NONE', *, *, #7870, .F. ) ;
#8922 = CARTESIAN_POINT ( 'NONE',  ( 208.8107687779841228, 4.427644383670616079, -14.00000000000005507 ) ) ;
#8923 = CARTESIAN_POINT ( 'NONE',  ( 220.2180084519553134, 35.41797800104779270, -14.00000000000005507 ) ) ;
#8924 = DIRECTION ( 'NONE',  ( 0.06808332454812035528, -0.1179237772655450794, 0.9906859460363316439 ) ) ;
#8925 = DIRECTION ( 'NONE',  ( -0.8660254037844354880, -0.5000000000000055511, 0.000000000000000000 ) ) ;
#8926 = ORIENTED_EDGE ( 'NONE', *, *, #17851, .T. ) ;
#8927 = CARTESIAN_POINT ( 'NONE',  ( 218.5981481562500335, 37.81172816583355711, -11.70804666182397291 ) ) ;
#8928 = CARTESIAN_POINT ( 'NONE',  ( 227.1024371503596342, 41.36244295655828296, -17.19244756328590285 ) ) ;
#8929 = LINE ( 'NONE', #13616, #1637 ) ;
#8930 = ORIENTED_EDGE ( 'NONE', *, *, #9256, .F. ) ;
#8931 = AXIS2_PLACEMENT_3D ( 'NONE', #3917, #18768, #752 ) ;
#8932 =( LENGTH_UNIT ( ) NAMED_UNIT ( * ) SI_UNIT ( .MILLI., .METRE. ) );
#8933 = CARTESIAN_POINT ( 'NONE',  ( 227.8089867185128412, 40.13866320645101382, -10.43865930680574827 ) ) ;
#8934 = LINE ( 'NONE', #676, #14956 ) ;
#8935 = CARTESIAN_POINT ( 'NONE',  ( -15.47785846381593089, 80.00000165566777355, -12.49590370130045258 ) ) ;
#8937 = ORIENTED_EDGE ( 'NONE', *, *, #15027, .T. ) ;
#8936 = ORIENTED_EDGE ( 'NONE', *, *, #18227, .T. ) ;
#8938 = VERTEX_POINT ( 'NONE', #19165 ) ;
#8939 = CARTESIAN_POINT ( 'NONE',  ( 1.500000000000001332, 7.960204194457796463E-16, -6.500000000000000888 ) ) ;
#8940 = CARTESIAN_POINT ( 'NONE',  ( -15.99999999999999289, 0.000000000000000000, 5.999999999999989342 ) ) ;
#8941 = VERTEX_POINT ( 'NONE', #12399 ) ;
#8942 = PLANE ( 'NONE',  #4626 ) ;
#8943 = FACE_OUTER_BOUND ( 'NONE', #280, .T. ) ;
#8944 = DIRECTION ( 'NONE',  ( 0.5000000000000045519, -0.8660254037844360431, -4.006172263299080561E-16 ) ) ;
#8945 = EDGE_LOOP ( 'NONE', ( #9111, #1235, #13673, #8655, #20742, #11974 ) ) ;
#8946 = ADVANCED_FACE ( 'NONE', ( #4430 ), #14205, .F. ) ;
#8947 = CARTESIAN_POINT ( 'NONE',  ( 225.5964691407864677, 42.99139017264894136, -13.49489896056980420 ) ) ;
#8948 = CARTESIAN_POINT ( 'NONE',  ( 208.3092871949524181, 11.56112132310344798, -15.97949511404853062 ) ) ;
#8949 = VERTEX_POINT ( 'NONE', #15888 ) ;
#8950 = CARTESIAN_POINT ( 'NONE',  ( 30.00000000000000000, 5.000000000000000000, 15.00000000000000000 ) ) ;
#8951 = PLANE ( 'NONE',  #12106 ) ;
#8952 = CARTESIAN_POINT ( 'NONE',  ( -34.33334827330879335, 64.25000000000000000, 2.147472525011941080 ) ) ;
#8953 = LINE ( 'NONE', #18193, #9799 ) ;
#8954 = DIRECTION ( 'NONE',  ( -0.1992005449231252778, 0.3450254647022572563, 0.9172113015054500496 ) ) ;
#8955 = VERTEX_POINT ( 'NONE', #8009 ) ;
#8956 = ORIENTED_EDGE ( 'NONE', *, *, #20138, .F. ) ;
#8957 = CARTESIAN_POINT ( 'NONE',  ( 0.000000000000000000, 5.000000000000000000, 30.00000000000000000 ) ) ;
#8958 = CARTESIAN_POINT ( 'NONE',  ( 226.1688508298258853, 42.97946189697395170, -13.95097276009431297 ) ) ;
#8959 = EDGE_CURVE ( 'NONE', #7333, #14290, #20331, .T. ) ;
#8960 = EDGE_LOOP ( 'NONE', ( #11870, #1570, #6970, #18957 ) ) ;
#8961 = EDGE_LOOP ( 'NONE', ( #3778, #2335 ) ) ;
#8962 = DIRECTION ( 'NONE',  ( 0.000000000000000000, -0.4999999999999983902, 0.8660254037844394848 ) ) ;
#8963 = CARTESIAN_POINT ( 'NONE',  ( 81.68654525303921332, 62.66781674343961583, 0.2910019319276673788 ) ) ;
#8964 = CARTESIAN_POINT ( 'NONE',  ( 195.2378745322255611, 8.138335620992030783, -7.515250618841283092 ) ) ;
#8965 = LINE ( 'NONE', #18416, #5275 ) ;
#8966 = FACE_OUTER_BOUND ( 'NONE', #5640, .T. ) ;
#8967 = CARTESIAN_POINT ( 'NONE',  ( 203.6269058993112253, 1.434739755226664970, -3.662783021451444299 ) ) ;
#8968 = EDGE_CURVE ( 'NONE', #3901, #19292, #20675, .T. ) ;
#8969 = EDGE_CURVE ( 'NONE', #18964, #2949, #7604, .T. ) ;
#8970 = LINE ( 'NONE', #4213, #19603 ) ;
#8971 = CIRCLE ( 'NONE', #7634, 12.47473710546057823 ) ;
#8972 = DIRECTION ( 'NONE',  ( 1.124692329640370702E-16, -7.528188728813031952E-17, 1.000000000000000000 ) ) ;
#8973 = CARTESIAN_POINT ( 'NONE',  ( -19.73795054555117545, 45.44664558820969802, -11.93297875370773298 ) ) ;
#8974 = CARTESIAN_POINT ( 'NONE',  ( 227.5312376355471145, 39.64027283883993391, -14.00000000000005507 ) ) ;
#8975 = CIRCLE ( 'NONE', #18128, 12.47473710546057823 ) ;
#8976 = CARTESIAN_POINT ( 'NONE',  ( 208.2331971963490389, 26.25586238970118558, -7.132002368301439077 ) ) ;
#8977 = PLANE ( 'NONE',  #9011 ) ;
#8978 = ADVANCED_FACE ( 'NONE', ( #4639 ), #17371, .T. ) ;
#8980 = VERTEX_POINT ( 'NONE', #10892 ) ;
#8979 = EDGE_LOOP ( 'NONE', ( #18406, #6520, #16445, #12629, #19704, #3136 ) ) ;
#8981 = CARTESIAN_POINT ( 'NONE',  ( 202.4229321854107013, 25.03106559388957209, -12.49995495381715749 ) ) ;
#8982 = CARTESIAN_POINT ( 'NONE',  ( 64.57205371728791476, 77.00255147951500589, -18.47244162738281048 ) ) ;
#8983 = ORIENTED_EDGE ( 'NONE', *, *, #2837, .F. ) ;
#8984 = ORIENTED_EDGE ( 'NONE', *, *, #6295, .T. ) ;
#8985 = CARTESIAN_POINT ( 'NONE',  ( 227.5647218214154464, 40.56174241872900410, -17.53429396590401623 ) ) ;
#8986 = CARTESIAN_POINT ( 'NONE',  ( 1.154989429455318684, 55.96508055892482503, -0.5199069304187589058 ) ) ;
#8987 = DIRECTION ( 'NONE',  ( -0.8660254037844361541, -0.5000000000000045519, 5.976026924694053325E-17 ) ) ;
#8988 = ADVANCED_FACE ( 'NONE', ( #6107 ), #11104, .F. ) ;
#8989 = EDGE_LOOP ( 'NONE', ( #6216, #14067, #16328, #9498 ) ) ;
#8990 = AXIS2_PLACEMENT_3D ( 'NONE', #8038, #9738, #117 ) ;
#8991 = ORIENTED_EDGE ( 'NONE', *, *, #18729, .F. ) ;
#8992 = DIRECTION ( 'NONE',  ( 0.5000000000000044409, -0.8660254037844360431, -0.000000000000000000 ) ) ;
#8993 = CIRCLE ( 'NONE', #5260, 12.47473710546057823 ) ;
#8994 = EDGE_CURVE ( 'NONE', #15958, #10655, #2410, .T. ) ;
#8995 = DIRECTION ( 'NONE',  ( -0.5000000000000054401, 0.8660254037844354880, -0.000000000000000000 ) ) ;
#8996 = FACE_BOUND ( 'NONE', #7712, .T. ) ;
#8997 = CARTESIAN_POINT ( 'NONE',  ( -14.37689184831195632, 19.83987654191486172, 12.39791892878506374 ) ) ;
#8998 = EDGE_CURVE ( 'NONE', #3962, #15581, #9429, .T. ) ;
#8999 = DIRECTION ( 'NONE',  ( -8.673617379884032514E-16, -0.7500000000000004441, -0.6614378277661471239 ) ) ;
#9000 = DIRECTION ( 'NONE',  ( -0.000000000000000000, -0.000000000000000000, 1.000000000000000000 ) ) ;
#9001 = CARTESIAN_POINT ( 'NONE',  ( 213.9089852488071983, 7.886307274364415143, -3.346771071760026750 ) ) ;
#9002 = AXIS2_PLACEMENT_3D ( 'NONE', #13631, #16801, #2279 ) ;
#9003 = EDGE_CURVE ( 'NONE', #470, #12613, #13775, .T. ) ;
#9004 = EDGE_LOOP ( 'NONE', ( #15820, #4603, #9366 ) ) ;
#9005 = CARTESIAN_POINT ( 'NONE',  ( -32.38807006469330929, 70.47620764902667645, 1.501429235142507590 ) ) ;
#9006 = DIRECTION ( 'NONE',  ( -0.5000000000000054401, 0.8660254037844354880, -0.000000000000000000 ) ) ;
#9007 = CARTESIAN_POINT ( 'NONE',  ( 226.0042218928572026, 43.26460758019940300, -13.97349461567471707 ) ) ;
#9008 = EDGE_CURVE ( 'NONE', #12336, #7292, #2061, .T. ) ;
#9009 = CIRCLE ( 'NONE', #17830, 3.619616396367202782 ) ;
#9010 = VERTEX_POINT ( 'NONE', #4737 ) ;
#9011 = AXIS2_PLACEMENT_3D ( 'NONE', #7380, #832, #12396 ) ;
#9012 = CARTESIAN_POINT ( 'NONE',  ( 80.14546250568827190, 56.34553042421615743, -2.766056647043495076 ) ) ;
#9013 = EDGE_LOOP ( 'NONE', ( #17695, #4146, #12309, #10682, #7785, #5931 ) ) ;
#9014 = VERTEX_POINT ( 'NONE', #11213 ) ;
#9015 = CARTESIAN_POINT ( 'NONE',  ( 220.8838919191435650, 34.26463400395766001, -10.33191597617941326 ) ) ;
#9016 = CARTESIAN_POINT ( 'NONE',  ( -14.99999999999999645, 0.000000000000000000, -28.99999999999999645 ) ) ;
#9017 = EDGE_CURVE ( 'NONE', #3518, #16137, #13246, .T. ) ;
#9018 =( NAMED_UNIT ( * ) PLANE_ANGLE_UNIT ( ) SI_UNIT ( $, .RADIAN. ) );
#9019 = LINE ( 'NONE', #13809, #14369 ) ;
#9020 = ORIENTED_EDGE ( 'NONE', *, *, #13779, .T. ) ;
#9021 = AXIS2_PLACEMENT_3D ( 'NONE', #8838, #5430, #11816 ) ;
#9022 = CARTESIAN_POINT ( 'NONE',  ( 211.6378943349726853, 6.575092323907928638, -2.216907231065539552 ) ) ;
#9023 = EDGE_CURVE ( 'NONE', #9807, #8913, #19065, .T. ) ;
#9024 = CARTESIAN_POINT ( 'NONE',  ( 201.2821527570645230, 0.5962021362443539196, -5.050953241461257903 ) ) ;
#9025 = CARTESIAN_POINT ( 'NONE',  ( 221.0007431456517395, 33.44439337337441032, -11.10922658182128764 ) ) ;
#9026 = DIRECTION ( 'NONE',  ( 0.5000000000000054401, -0.8660254037844354880, 0.000000000000000000 ) ) ;
#9027 = CARTESIAN_POINT ( 'NONE',  ( 228.8082804645358408, 38.40783566665349724, -17.19244756328599522 ) ) ;
#9028 = EDGE_CURVE ( 'NONE', #7589, #1433, #18311, .T. ) ;
#9029 = LINE ( 'NONE', #2366, #9548 ) ;
#9030 = PLANE ( 'NONE',  #10763 ) ;
#9031 = B_SPLINE_CURVE_WITH_KNOTS ( 'NONE', 3,
 ( #13021, #20946, #12916, #9500 ),
 .UNSPECIFIED., .F., .F.,
 ( 4, 4 ),
 ( 0.0001038643694185014657, 0.0009578501073958695404 ),
 .UNSPECIFIED. ) ;
#9032 = ORIENTED_EDGE ( 'NONE', *, *, #1655, .T. ) ;
#9033 = CARTESIAN_POINT ( 'NONE',  ( 89.99529059433416478, 168.0799536996104848, 26.00000000000001066 ) ) ;
#9034 = ADVANCED_FACE ( 'NONE', ( #4943 ), #7130, .T. ) ;
#9035 = VECTOR ( 'NONE', #20853, 1000.000000000000227 ) ;
#9036 = DIRECTION ( 'NONE',  ( -0.5000000000000043299, 0.8660254037844361541, 1.272130549049658700E-16 ) ) ;
#9037 = DIRECTION ( 'NONE',  ( 0.5000000000000054401, -0.8660254037844354880, 0.000000000000000000 ) ) ;
#9039 = VERTEX_POINT ( 'NONE', #17782 ) ;
#9038 = ORIENTED_EDGE ( 'NONE', *, *, #16424, .F. ) ;
#9040 = ORIENTED_EDGE ( 'NONE', *, *, #6782, .F. ) ;
#9041 = ORIENTED_EDGE ( 'NONE', *, *, #10063, .F. ) ;
#9042 = CARTESIAN_POINT ( 'NONE',  ( -14.22556875492139561, 10.42203463021438559, 12.37434949811833818 ) ) ;
#9043 = DIRECTION ( 'NONE',  ( 0.4999999999999995004, -0.8660254037844390407, 0.000000000000000000 ) ) ;
#9044 = CARTESIAN_POINT ( 'NONE',  ( -25.10457607615188991, 79.90025503832140430, -10.76317361290839436 ) ) ;
#9045 = ORIENTED_EDGE ( 'NONE', *, *, #12093, .T. ) ;
#9046 = LINE ( 'NONE', #20285, #8336 ) ;
#9047 = DIRECTION ( 'NONE',  ( 0.3841106397986914223, -0.6652991438591137063, 0.6401843996644798196 ) ) ;
#9048 = ORIENTED_EDGE ( 'NONE', *, *, #6035, .F. ) ;
#9049 = AXIS2_PLACEMENT_3D ( 'NONE', #2608, #17434, #9353 ) ;
#9050 = B_SPLINE_CURVE_WITH_KNOTS ( 'NONE', 3,
 ( #9547, #19504, #16046, #3396 ),
 .UNSPECIFIED., .F., .F.,
 ( 4, 4 ),
 ( 2.004673356279735398E-07, 4.934226812140153520E-05 ),
 .UNSPECIFIED. ) ;
#9051 = B_SPLINE_CURVE_WITH_KNOTS ( 'NONE', 3,
 ( #7125, #9129, #5419, #13820 ),
 .UNSPECIFIED., .F., .F.,
 ( 4, 4 ),
 ( 6.440264276912068765E-07, 0.0008546297644052478458 ),
 .UNSPECIFIED. ) ;
#9052 = CYLINDRICAL_SURFACE ( 'NONE', #10908, 5.999999999999998224 ) ;
#9053 = ORIENTED_EDGE ( 'NONE', *, *, #6924, .T. ) ;
#9054 = CARTESIAN_POINT ( 'NONE',  ( 200.4885253383106374, 7.045802359903295731, -24.25943249057081630 ) ) ;
#9055 = DIRECTION ( 'NONE',  ( -0.5000000000000046629, 0.8660254037844359321, 0.000000000000000000 ) ) ;
#9056 = LINE ( 'NONE', #9157, #10125 ) ;
#9057 = CARTESIAN_POINT ( 'NONE',  ( 228.2110680366503743, 39.11576885869645537, -17.62796654520765571 ) ) ;
#9058 = CARTESIAN_POINT ( 'NONE',  ( -34.00000000000000711, 65.00000000000000000, -12.50000000000000000 ) ) ;
#9059 = ORIENTED_EDGE ( 'NONE', *, *, #12608, .T. ) ;
#9060 = VERTEX_POINT ( 'NONE', #9705 ) ;
#9061 = CARTESIAN_POINT ( 'NONE',  ( 208.8107687779840944, 4.427644383670621409, -14.00000000000005507 ) ) ;
#9062 = ORIENTED_EDGE ( 'NONE', *, *, #744, .F. ) ;
#9063 = ORIENTED_EDGE ( 'NONE', *, *, #12117, .F. ) ;
#9064 = AXIS2_PLACEMENT_3D ( 'NONE', #12739, #2992, #7852 ) ;
#9065 = ADVANCED_FACE ( 'NONE', ( #6848 ), #14625, .F. ) ;
#9066 = CARTESIAN_POINT ( 'NONE',  ( -20.99999999999998934, 14.77053021905504693, 11.45643923738960446 ) ) ;
#9067 = PRODUCT_DEFINITION_SHAPE ( 'NONE', 'NONE',  #19727 ) ;
#9068 = CARTESIAN_POINT ( 'NONE',  ( 79.53442306383087157, 49.97558790125707873, -9.251858224647309115 ) ) ;
#9069 = CARTESIAN_POINT ( 'NONE',  ( 221.6237444509601460, 32.57124166020339118, -15.87804042560544637 ) ) ;
#9070 = FACE_OUTER_BOUND ( 'NONE', #9403, .T. ) ;
#9071 = ORIENTED_EDGE ( 'NONE', *, *, #9871, .F. ) ;
#9072 = CYLINDRICAL_SURFACE ( 'NONE', #9452, 4.999999999999973355 ) ;
#9073 = EDGE_CURVE ( 'NONE', #12607, #1135, #13913, .T. ) ;
#9074 = CIRCLE ( 'NONE', #634, 8.000000000000000000 ) ;
#9075 = CARTESIAN_POINT ( 'NONE',  ( -14.15118760488712013, 49.50739088371899754, -12.36866518513531332 ) ) ;
#9076 = LINE ( 'NONE', #15576, #15701 ) ;
#9077 = CARTESIAN_POINT ( 'NONE',  ( 86.00000000000000000, 65.00000000000000000, -12.50000000000000000 ) ) ;
#9078 =( BOUNDED_SURFACE ( )  B_SPLINE_SURFACE ( 3, 2, ( 
 ( #1798, #4755, #17597 ),
 ( #6332, #17494, #3070 ),
 ( #17912, #19477, #7831 ),
 ( #19184, #11237, #17707 ),
 ( #4656, #9520, #1483 ),
 ( #7928, #9624, #4863 ),
 ( #20859, #1687, #17801 ),
 ( #14537, #8237, #201 ),
 ( #16119, #11334, #1585 ),
 ( #12623, #8026, #3272 ),
 ( #9724, #8134, #107 ),
 ( #13038, #16522, #20010 ),
 ( #19691, #5162, #520 ),
 ( #621, #19582, #11652 ),
 ( #18013, #10027, #5264 ),
 ( #2318, #13137, #417 ),
 ( #3483, #8774, #8563 ),
 ( #8449, #9928, #14952 ),
 ( #15062, #8670, #18213 ),
 ( #6863, #13348, #301 ),
 ( #10131, #16422, #5366 ),
 ( #6746, #5474, #13243 ),
 ( #1898, #3678, #3582 ),
 ( #19795, #2001, #11753 ),
 ( #8347, #14851, #18114 ),
 ( #16624, #2113, #6965 ),
 ( #13452, #15270, #5059 ),
 ( #6642, #3895, #19900 ),
 ( #11538, #11858, #18322 ),
 ( #10348, #3791, #10241 ),
 ( #16732, #2212, #15167 ),
 ( #7074, #13558, #18426 ),
 ( #11967, #16835, #18743 ),
 ( #18944, #20426, #4003 ),
 ( #2420, #15685, #8876 ),
 ( #7595, #5577, #14087 ),
 ( #13870, #5791, #5681 ),
 ( #12171, #16937, #1150 ),
 ( #20320, #15575, #10452 ),
 ( #10773, #5891, #20524 ),
 ( #5995, #12488, #20116 ),
 ( #12391, #2528, #4112 ),
 ( #13984, #4216, #18637 ),
 ( #8973, #4422, #13663 ),
 ( #10567, #10882, #9178 ),
 ( #2736, #18846, #4320 ),
 ( #17364, #15375, #17250 ),
 ( #2841, #827, #7180 ),
 ( #9279, #17150, #7274 ),
 ( #2634, #15475, #18534 ),
 ( #12288, #13764, #726 ),
 ( #932, #7376, #10664 ),
 ( #12067, #9075, #20213 ),
 ( #17050, #1038, #7490 ),
 ( #6513, #8003, #1250 ),
 ( #14509, #8102, #20935 ),
 ( #13012, #14616, #16092 ),
 ( #1662, #4729, #11097 ),
 ( #15992, #15879, #17887 ),
 ( #1558, #11409, #19451 ),
 ( #12594, #15782, #17570 ),
 ( #20627, #17773, #78 ),
 ( #3242, #12698, #14303 ),
 ( #9382, #14198, #11308 ),
 ( #1457, #4630, #3349 ),
 ( #4934, #7903, #20738 ),
 ( #9489, #7697, #6206 ),
 ( #9594, #6099, #6408 ),
 ( #9697, #6306, #12906 ),
 ( #19359, #19261, #19057 ),
 ( #3040, #19156, #16192 ),
 ( #4835, #1352, #11203 ),
 ( #4530, #10997, #17465 ),
 ( #20830, #2943, #14402 ),
 ( #7801, #12801, #17678 ),
 ( #3148, #1870, #19664 ),
 ( #5034, #5137, #2188 ),
 ( #8319, #14823, #3654 ),
 ( #8537, #595, #3454 ),
 ( #3553, #7045, #5236 ),
 ( #9903, #11727, #9998 ),
 ( #11625, #13529, #18189 ),
 ( #387, #16492, #18088 ),
 ( #16396, #15038, #13323 ),
 ( #16596, #11510, #273 ),
 ( #6718, #19979, #19556 ),
 ( #13214, #14922, #1973 ),
 ( #8421, #10107, #173 ),
 ( #6839, #16710, #19770 ),
 ( #6617, #2083, #496 ),
 ( #8212, #6935, #5442 ),
 ( #16292, #13426, #17988 ),
 ( #19871, #14719, #11830 ),
 ( #5337, #18290, #3764 ),
 ( #10216, #8640, #13111 ),
 ( #15140, #11941, #18401 ),
 ( #9802, #1768, #17024 ),
 ( #5871, #18608, #10321 ) ),
 .UNSPECIFIED., .F., .F., .T. ) 
 B_SPLINE_SURFACE_WITH_KNOTS ( ( 4, 2, 2, 2, 2, 2, 2, 2, 2, 2, 2, 2, 2, 2, 2, 2, 2, 2, 2, 2, 2, 2, 2, 2, 2, 2, 2, 2, 2, 2, 2, 2, 2, 2, 2, 2, 2, 2, 2, 2, 2, 2, 2, 2, 2, 2, 2, 2, 4 ),
 ( 3, 3 ),
 ( 0.05371843306266368967, 0.05659148630217877840, 0.05802801292193632277, 0.05946453954169386713, 0.06233759278120895586, 0.06377411940096650023, 0.06521064602072404459, 0.06808369926023913332, 0.06952022587999667769, 0.07095675249975422205, 0.07382980573926931078, 0.07526633235902685515, 0.07670285897878439951, 0.07957591221829948824, 0.08101243883805703261, 0.08244896545781457697, 0.08388549207757212134, 0.08532201869732966570, 0.08819507193684475443, 0.08963159855660229880, 0.09106812517635984316, 0.09394117841587493190, 0.09537770503563247626, 0.09681423165539002063, 0.09968728489490510936, 0.1011238115146626537, 0.1025603381344201981, 0.1054333913739352868, 0.1068699179936928312, 0.1083064446134503755, 0.1111794978529654643, 0.1126160244727230086, 0.1140525510924805530, 0.1169256043319956417, 0.1183621309517531861, 0.1197986575715107305, 0.1226717108110258192, 0.1241082374307833636, 0.1255447640505409079, 0.1269812906702984523, 0.1284178172900559967, 0.1312908705295710854, 0.1327273971493286298, 0.1341639237690861741, 0.1370369770086012629, 0.1384735036283588072, 0.1399100302481163516, 0.1427830834876314403, 0.1456561367271465290 ),
 ( 0.000000000000000000, 1.000000000000000000 ),
 .UNSPECIFIED. ) 
 GEOMETRIC_REPRESENTATION_ITEM ( )  RATIONAL_B_SPLINE_SURFACE ( (
 ( 1.000000000000000000, 0.8451295721185223542, 1.000000000000000000),
 ( 1.000000000000000000, 0.8449004303875792266, 1.000000000000000000),
 ( 1.000000000000000000, 0.8430801628613031617, 1.000000000000000000),
 ( 1.000000000000000000, 0.8379707563242198010, 1.000000000000000000),
 ( 1.000000000000000000, 0.8358658383963908367, 1.000000000000000000),
 ( 1.000000000000000000, 0.8309676740331579659, 1.000000000000000000),
 ( 1.000000000000000000, 0.8281679717263343843, 1.000000000000000000),
 ( 1.000000000000000000, 0.8188015739685772232, 1.000000000000000000),
 ( 1.000000000000000000, 0.8112657144558387268, 1.000000000000000000),
 ( 1.000000000000000000, 0.7983672344561800749, 1.000000000000000000),
 ( 1.000000000000000000, 0.7937839858167325957, 1.000000000000000000),
 ( 1.000000000000000000, 0.7842772446598291758, 1.000000000000000000),
 ( 1.000000000000000000, 0.7793499137115288411, 1.000000000000000000),
 ( 1.000000000000000000, 0.7641988213884888248, 1.000000000000000000),
 ( 1.000000000000000000, 0.7535972611492264273, 1.000000000000000000),
 ( 1.000000000000000000, 0.7376610632163976833, 1.000000000000000000),
 ( 1.000000000000000000, 0.7323451700871047576, 1.000000000000000000),
 ( 1.000000000000000000, 0.7218574730905190640, 1.000000000000000000),
 ( 1.000000000000000000, 0.7167041927396170520, 1.000000000000000000),
 ( 1.000000000000000000, 0.7019988979607418855, 1.000000000000000000),
 ( 1.000000000000000000, 0.6931069249354639972, 1.000000000000000000),
 ( 1.000000000000000000, 0.6821959854549815017, 1.000000000000000000),
 ( 1.000000000000000000, 0.6789533902147232292, 1.000000000000000000),
 ( 1.000000000000000000, 0.6735202903929765617, 1.000000000000000000),
 ( 1.000000000000000000, 0.6713489072053013818, 1.000000000000000000),
 ( 1.000000000000000000, 0.6665638323410731925, 1.000000000000000000),
 ( 1.000000000000000000, 0.6656972691007314591, 1.000000000000000000),
 ( 1.000000000000000000, 0.6679527106063430919, 1.000000000000000000),
 ( 1.000000000000000000, 0.6693061893886460556, 1.000000000000000000),
 ( 1.000000000000000000, 0.6730365072794786130, 1.000000000000000000),
 ( 1.000000000000000000, 0.6754117021867901416, 1.000000000000000000),
 ( 1.000000000000000000, 0.6810047018611226077, 1.000000000000000000),
 ( 1.000000000000000000, 0.6842223828699847132, 1.000000000000000000),
 ( 1.000000000000000000, 0.6913184916867489704, 1.000000000000000000),
 ( 1.000000000000000000, 0.6952162037222894275, 1.000000000000000000),
 ( 1.000000000000000000, 0.7074730050970403639, 1.000000000000000000),
 ( 1.000000000000000000, 0.7163322597878015729, 1.000000000000000000),
 ( 1.000000000000000000, 0.7295517996625942025, 1.000000000000000000),
 ( 1.000000000000000000, 0.7339499638009396865, 1.000000000000000000),
 ( 1.000000000000000000, 0.7425745160330512462, 1.000000000000000000),
 ( 1.000000000000000000, 0.7467701689946989463, 1.000000000000000000),
 ( 1.000000000000000000, 0.7587200212276741240, 1.000000000000000000),
 ( 1.000000000000000000, 0.7658780977019831182, 1.000000000000000000),
 ( 1.000000000000000000, 0.7748278484315241910, 1.000000000000000000),
 ( 1.000000000000000000, 0.7775215145640017589, 1.000000000000000000),
 ( 1.000000000000000000, 0.7821966049398736409, 1.000000000000000000),
 ( 1.000000000000000000, 0.7841643293397753123, 1.000000000000000000),
 ( 1.000000000000000000, 0.7889180347041169217, 1.000000000000000000),
 ( 1.000000000000000000, 0.7905538983596147595, 1.000000000000000000),
 ( 1.000000000000000000, 0.7905770084924903518, 1.000000000000000000),
 ( 1.000000000000000000, 0.7901767721866111982, 1.000000000000000000),
 ( 1.000000000000000000, 0.7885605096290441152, 1.000000000000000000),
 ( 1.000000000000000000, 0.7873530734365258299, 1.000000000000000000),
 ( 1.000000000000000000, 0.7826096900989555349, 1.000000000000000000),
 ( 1.000000000000000000, 0.7779500639155249031, 1.000000000000000000),
 ( 1.000000000000000000, 0.7690412136372090091, 1.000000000000000000),
 ( 1.000000000000000000, 0.7657396504301140494, 1.000000000000000000),
 ( 1.000000000000000000, 0.7586220519610614721, 1.000000000000000000),
 ( 1.000000000000000000, 0.7548291205712890362, 1.000000000000000000),
 ( 1.000000000000000000, 0.7429250358377615937, 1.000000000000000000),
 ( 1.000000000000000000, 0.7342788820070000888, 1.000000000000000000),
 ( 1.000000000000000000, 0.7210645840206886259, 1.000000000000000000),
 ( 1.000000000000000000, 0.7166062187610443557, 1.000000000000000000),
 ( 1.000000000000000000, 0.7078513950284187617, 1.000000000000000000),
 ( 1.000000000000000000, 0.7035928640278642510, 1.000000000000000000),
 ( 1.000000000000000000, 0.6914457770771308409, 1.000000000000000000),
 ( 1.000000000000000000, 0.6841809009208725811, 1.000000000000000000),
 ( 1.000000000000000000, 0.6756975108818989995, 1.000000000000000000),
 ( 1.000000000000000000, 0.6732685451421130951, 1.000000000000000000),
 ( 1.000000000000000000, 0.6694443308151706296, 1.000000000000000000),
 ( 1.000000000000000000, 0.6680762773069750526, 1.000000000000000000),
 ( 1.000000000000000000, 0.6657056734595532266, 1.000000000000000000),
 ( 1.000000000000000000, 0.6664547459774202709, 1.000000000000000000),
 ( 1.000000000000000000, 0.6711610830150476215, 1.000000000000000000),
 ( 1.000000000000000000, 0.6733389247384340415, 1.000000000000000000),
 ( 1.000000000000000000, 0.6787002311037058089, 1.000000000000000000),
 ( 1.000000000000000000, 0.6818858631847106722, 1.000000000000000000),
 ( 1.000000000000000000, 0.6891021881274688177, 1.000000000000000000),
 ( 1.000000000000000000, 0.6931327393535783310, 1.000000000000000000),
 ( 1.000000000000000000, 0.7018714184841962078, 1.000000000000000000),
 ( 1.000000000000000000, 0.7066008739865929922, 1.000000000000000000),
 ( 1.000000000000000000, 0.7213821357138887613, 1.000000000000000000),
 ( 1.000000000000000000, 0.7319733230681478853, 1.000000000000000000),
 ( 1.000000000000000000, 0.7479842531354111701, 1.000000000000000000),
 ( 1.000000000000000000, 0.7533449566548310328, 1.000000000000000000),
 ( 1.000000000000000000, 0.7639785367744996725, 1.000000000000000000),
 ( 1.000000000000000000, 0.7692354322323328164, 1.000000000000000000),
 ( 1.000000000000000000, 0.7844906279380156056, 1.000000000000000000),
 ( 1.000000000000000000, 0.7940371516267079599, 1.000000000000000000),
 ( 1.000000000000000000, 0.8069106371822711843, 1.000000000000000000),
 ( 1.000000000000000000, 0.8109620220656993395, 1.000000000000000000),
 ( 1.000000000000000000, 0.8185080840883726117, 1.000000000000000000),
 ( 1.000000000000000000, 0.8220058205555477171, 1.000000000000000000),
 ( 1.000000000000000000, 0.8314117683381576640, 1.000000000000000000),
 ( 1.000000000000000000, 0.8362949755366669846, 1.000000000000000000),
 ( 1.000000000000000000, 0.8430419324072143672, 1.000000000000000000),
 ( 1.000000000000000000, 0.8449066468994074208, 1.000000000000000000),
 ( 1.000000000000000000, 0.8451313959173227808, 1.000000000000000000) ) ) 
 REPRESENTATION_ITEM ( '' )  SURFACE ( )  );
#9079 = CARTESIAN_POINT ( 'NONE',  ( 229.5134838794282643, 37.18638752238859269, -15.84136033874758454 ) ) ;
#9081 = ORIENTED_EDGE ( 'NONE', *, *, #12114, .F. ) ;
#9080 = VERTEX_POINT ( 'NONE', #13332 ) ;
#9082 = DIRECTION ( 'NONE',  ( -0.8660254037844357100, -0.5000000000000051070, 0.000000000000000000 ) ) ;
#9083 = DIRECTION ( 'NONE',  ( 0.5000000000000054401, -0.8660254037844354880, 0.000000000000000000 ) ) ;
#9084 = EDGE_CURVE ( 'NONE', #9311, #17484, #10444, .T. ) ;
#9085 = LINE ( 'NONE', #7811, #9409 ) ;
#9086 = ORIENTED_EDGE ( 'NONE', *, *, #19823, .F. ) ;
#9087 = EDGE_CURVE ( 'NONE', #1135, #15273, #15066, .T. ) ;
#9088 = CARTESIAN_POINT ( 'NONE',  ( 218.5840739019945147, 36.11668090005408516, -18.00871210835852310 ) ) ;
#9089 = CARTESIAN_POINT ( 'NONE',  ( 229.4124125612959801, 36.70848904807888857, -15.54732812283888244 ) ) ;
#9090 = CARTESIAN_POINT ( 'NONE',  ( -25.87449106562930368, 50.06942782642894230, -13.97928078101991289 ) ) ;
#9091 = CARTESIAN_POINT ( 'NONE',  ( -28.06278917795930283, 9.095778419061115727, -3.341700078353888159 ) ) ;
#9092 = ORIENTED_EDGE ( 'NONE', *, *, #16231, .F. ) ;
#9093 = AXIS2_PLACEMENT_3D ( 'NONE', #1503, #9543, #9846 ) ;
#9094 = ORIENTED_EDGE ( 'NONE', *, *, #4556, .F. ) ;
#9095 = PLANE ( 'NONE',  #17863 ) ;
#9096 = CARTESIAN_POINT ( 'NONE',  ( 10.49211908931699178, -10.00000000000000000, -5.000000000000000000 ) ) ;
#9097 = CARTESIAN_POINT ( 'NONE',  ( -46.99999999999998579, 65.00000000000000000, -12.50000000000000000 ) ) ;
#9098 = CARTESIAN_POINT ( 'NONE',  ( 229.3902669520996653, 37.07333642490806369, -12.03677242795827951 ) ) ;
#9099 = PRODUCT_RELATED_PRODUCT_CATEGORY ( 'part', '', ( #7367 ) ) ;
#9100 = FACE_OUTER_BOUND ( 'NONE', #13183, .T. ) ;
#9101 = CARTESIAN_POINT ( 'NONE',  ( 205.8264633344831225, 9.596613037118636669, -14.00000000000005507 ) ) ;
#9102 = CARTESIAN_POINT ( 'NONE',  ( 220.2180084519553134, 35.41797800104779270, -14.00000000000005507 ) ) ;
#9103 = CARTESIAN_POINT ( 'NONE',  ( -28.88216758755841695, 75.18040026313910573, -1.430629151363568718 ) ) ;
#9104 = CARTESIAN_POINT ( 'NONE',  ( 62.61279602124705690, 155.5078255381764336, 41.00000000000001421 ) ) ;
#9105 = DIRECTION ( 'NONE',  ( -0.8660254037844355990, -0.5000000000000054401, -2.753366626804969431E-14 ) ) ;
#9106 = CIRCLE ( 'NONE', #12181, 14.99999999999999645 ) ;
#9107 = ORIENTED_EDGE ( 'NONE', *, *, #4060, .T. ) ;
#9108 = CARTESIAN_POINT ( 'NONE',  ( 82.94070292489149665, 62.10228613400511932, 0.3639711883102479395 ) ) ;
#9109 = EDGE_CURVE ( 'NONE', #20898, #17666, #15553, .T. ) ;
#9110 = VERTEX_POINT ( 'NONE', #11519 ) ;
#9111 = ORIENTED_EDGE ( 'NONE', *, *, #5262, .F. ) ;
#9112 = CARTESIAN_POINT ( 'NONE',  ( -4.701390418375632763, 64.25000000000000000, 5.347094680480811490 ) ) ;
#9113 = B_SPLINE_CURVE_WITH_KNOTS ( 'NONE', 3,
 ( #12784, #8082, #14592, #16376 ),
 .UNSPECIFIED., .F., .F.,
 ( 4, 4 ),
 ( 2.602969390140976553E-05, 0.0006986804859590750897 ),
 .UNSPECIFIED. ) ;
#9114 = CARTESIAN_POINT ( 'NONE',  ( 205.0662616026534693, 10.91332106064940888, -14.00000000000005507 ) ) ;
#9115 = APPLICATION_PROTOCOL_DEFINITION ( 'draft international standard', 'automotive_design', 1998, #7405 ) ;
#9116 = DIRECTION ( 'NONE',  ( -0.1997192025788092906, -0.1153079353712144900, 0.9730448705798270259 ) ) ;
#9117 = EDGE_CURVE ( 'NONE', #7191, #9345, #12571, .T. ) ;
#9118 = ORIENTED_EDGE ( 'NONE', *, *, #16931, .T. ) ;
#9119 = LINE ( 'NONE', #20468, #6347 ) ;
#9120 = DIRECTION ( 'NONE',  ( -0.8660254037844370423, -0.5000000000000026645, 0.000000000000000000 ) ) ;
#9121 = DIRECTION ( 'NONE',  ( 0.000000000000000000, -0.9123518090004750780, 0.4094071037653847500 ) ) ;
#9122 = CARTESIAN_POINT ( 'NONE',  ( 105.7973891242897650, 30.70991617951901986, -12.50000000000000000 ) ) ;
#9123 = CIRCLE ( 'NONE', #3038, 12.00000000000002487 ) ;
#9124 = CARTESIAN_POINT ( 'NONE',  ( 218.7787453705537928, 10.18265835266665675, -11.24974199967301836 ) ) ;
#9125 = B_SPLINE_CURVE_WITH_KNOTS ( 'NONE', 3,
 ( #15688, #1152, #17573, #19264 ),
 .UNSPECIFIED., .F., .F.,
 ( 4, 4 ),
 ( 9.760775661998381803E-05, 0.0009515934945975094679 ),
 .UNSPECIFIED. ) ;
#9126 = EDGE_CURVE ( 'NONE', #9807, #15362, #8328, .T. ) ;
#9127 = CARTESIAN_POINT ( 'NONE',  ( 40.35427444295665822, 174.0607158131434176, 11.00000000000001243 ) ) ;
#9128 = CARTESIAN_POINT ( 'NONE',  ( 225.8710342809365557, 42.51582939992156440, -11.94979443502192318 ) ) ;
#9129 = CARTESIAN_POINT ( 'NONE',  ( 199.0720388946177195, -0.6798076971790223411, -19.52417598135467713 ) ) ;
#9130 = EDGE_LOOP ( 'NONE', ( #3867, #5887, #11048, #13853, #16717, #15358 ) ) ;
#9131 = FACE_BOUND ( 'NONE', #19422, .T. ) ;
#9132 = EDGE_CURVE ( 'NONE', #18220, #5668, #19459, .T. ) ;
#9133 = CARTESIAN_POINT ( 'NONE',  ( 228.8686933265739185, 37.97672844420654314, -17.05667259846724448 ) ) ;
#9134 = LINE ( 'NONE', #12347, #9535 ) ;
#9135 = AXIS2_PLACEMENT_3D ( 'NONE', #12548, #4489, #1516 ) ;
#9136 = LINE ( 'NONE', #7132, #10435 ) ;
#9138 = ORIENTED_EDGE ( 'NONE', *, *, #5262, .T. ) ;
#9137 = ORIENTED_EDGE ( 'NONE', *, *, #8901, .T. ) ;
#9139 = AXIS2_PLACEMENT_3D ( 'NONE', #13619, #2370, #3738 ) ;
#9140 = CARTESIAN_POINT ( 'NONE',  ( -11.51245442718898992, 12.87030402641002702, 11.66749078037026521 ) ) ;
#9141 = DIRECTION ( 'NONE',  ( -0.04526787302125637180, 0.07840625602339144906, -0.9958932064677044060 ) ) ;
#9142 = VECTOR ( 'NONE', #12003, 1000.000000000000000 ) ;
#9143 = EDGE_CURVE ( 'NONE', #19333, #6944, #12915, .T. ) ;
#9144 = DIRECTION ( 'NONE',  ( 0.4999999999999995004, -0.8660254037844390407, 0.000000000000000000 ) ) ;
#9145 = EDGE_CURVE ( 'NONE', #122, #10810, #3663, .T. ) ;
#9146 = ORIENTED_EDGE ( 'NONE', *, *, #2694, .T. ) ;
#9147 = ORIENTED_EDGE ( 'NONE', *, *, #12767, .F. ) ;
#9148 = CIRCLE ( 'NONE', #11876, 5.000000000000005329 ) ;
#9149 = CARTESIAN_POINT ( 'NONE',  ( 0.000000000000000000, 3.518949890710767026, -4.987329993433320396E-15 ) ) ;
#9150 = CARTESIAN_POINT ( 'NONE',  ( 201.4958824572256333, 7.627400263678961068, -2.990331769139143780 ) ) ;
#9151 = CONICAL_SURFACE ( 'NONE', #18308, 13.07248899748297433, 0.6693469023067423196 ) ;
#9152 = ADVANCED_FACE ( 'NONE', ( #8220 ), #16405, .F. ) ;
#9153 = ORIENTED_EDGE ( 'NONE', *, *, #19437, .T. ) ;
#9154 = CARTESIAN_POINT ( 'NONE',  ( 1.500000000000001332, 0.000000000000000000, 0.000000000000000000 ) ) ;
#9155 = LINE ( 'NONE', #908, #13577 ) ;
#9156 = DIRECTION ( 'NONE',  ( 0.3412765716093286716, -0.5911083614602702374, 0.7308359642781253607 ) ) ;
#9157 = CARTESIAN_POINT ( 'NONE',  ( 32.39721438298032297, 261.8427481158985870, -22.00000000000000355 ) ) ;
#9158 = CARTESIAN_POINT ( 'NONE',  ( 4.000000000000000000, 3.732111120401558708E-16, -3.047499999999999876 ) ) ;
#9160 = ORIENTED_EDGE ( 'NONE', *, *, #13405, .F. ) ;
#9159 = EDGE_LOOP ( 'NONE', ( #6414, #11892, #5145, #60 ) ) ;
#9161 = EDGE_LOOP ( 'NONE', ( #3046, #2119, #1726, #12684 ) ) ;
#9162 = CARTESIAN_POINT ( 'NONE',  ( 45.00000000000000000, -10.00000000000000000, 0.000000000000000000 ) ) ;
#9163 = EDGE_CURVE ( 'NONE', #6425, #12475, #16302, .T. ) ;
#9164 = AXIS2_PLACEMENT_3D ( 'NONE', #20864, #19291, #13326 ) ;
#9165 = VECTOR ( 'NONE', #6953, 1000.000000000000000 ) ;
#9166 = ORIENTED_EDGE ( 'NONE', *, *, #17534, .F. ) ;
#9167 = ORIENTED_EDGE ( 'NONE', *, *, #15707, .F. ) ;
#9168 = CARTESIAN_POINT ( 'NONE',  ( 200.4167038695724443, 7.004336215593725434, -24.38552490958304020 ) ) ;
#9169 = CARTESIAN_POINT ( 'NONE',  ( 227.1736134143502568, 40.91269297506731561, -10.51396113533821364 ) ) ;
#9170 = AXIS2_PLACEMENT_3D ( 'NONE', #16997, #10191, #15424 ) ;
#9171 = CARTESIAN_POINT ( 'NONE',  ( 200.4154830772234561, 6.826621486618904555, -24.52223341984387872 ) ) ;
#9172 = AXIS2_PLACEMENT_3D ( 'NONE', #9061, #7991, #11604 ) ;
#9173 = CARTESIAN_POINT ( 'NONE',  ( 205.8264633344831225, 9.596613037118636669, -14.00000000000005507 ) ) ;
#9174 = DIRECTION ( 'NONE',  ( -0.5000000000000049960, 0.8660254037844357100, -0.000000000000000000 ) ) ;
#9175 = ORIENTED_EDGE ( 'NONE', *, *, #5295, .T. ) ;
#9176 = CARTESIAN_POINT ( 'NONE',  ( 28.51452848080068847, 214.5677573683055357, -19.00000000000000000 ) ) ;
#9177 = CARTESIAN_POINT ( 'NONE',  ( 218.9002013747199555, 37.08263844404898180, -11.10922658182122902 ) ) ;
#9178 = CARTESIAN_POINT ( 'NONE',  ( -20.76827921581725178, 50.35794673965182966, -15.75863071056655329 ) ) ;
#9179 = LINE ( 'NONE', #20214, #4831 ) ;
#9180 = VECTOR ( 'NONE', #7917, 1000.000000000000000 ) ;
#9181 = DIRECTION ( 'NONE',  ( 0.000000000000000000, 0.000000000000000000, -1.000000000000000000 ) ) ;
#9182 = AXIS2_PLACEMENT_3D ( 'NONE', #106, #1584, #6536 ) ;
#9183 = CARTESIAN_POINT ( 'NONE',  ( 208.4761278624580711, 5.007259451653140125, -14.00000000000005507 ) ) ;
#9185 = VERTEX_POINT ( 'NONE', #5148 ) ;
#9184 = ORIENTED_EDGE ( 'NONE', *, *, #7302, .F. ) ;
#9186 = DIRECTION ( 'NONE',  ( 0.000000000000000000, 0.000000000000000000, -1.000000000000000000 ) ) ;
#9187 = LINE ( 'NONE', #5900, #11540 ) ;
#9188 = CARTESIAN_POINT ( 'NONE',  ( -3.532373732925984111, 79.99999999989431387, -0.9530258780636241545 ) ) ;
#9189 = VERTEX_POINT ( 'NONE', #6625 ) ;
#9190 = ORIENTED_EDGE ( 'NONE', *, *, #15245, .T. ) ;
#9191 = CARTESIAN_POINT ( 'NONE',  ( 218.7131701895986851, 37.40658595927892094, -16.57782486433068669 ) ) ;
#9192 = CARTESIAN_POINT ( 'NONE',  ( -14.99999999999999645, 5.000000000000000000, 30.00000000000000000 ) ) ;
#9193 = CARTESIAN_POINT ( 'NONE',  ( -27.89607850596237171, 49.99668640821654719, -12.77299574469434518 ) ) ;
#9194 = CARTESIAN_POINT ( 'NONE',  ( -27.75180011566605742, 9.360503832615256314, -4.272254040061502778 ) ) ;
#9195 = ORIENTED_EDGE ( 'NONE', *, *, #4739, .F. ) ;
#9196 = AXIS2_PLACEMENT_3D ( 'NONE', #11064, #3008, #6579 ) ;
#9197 = VERTEX_POINT ( 'NONE', #8548 ) ;
#9198 = DIRECTION ( 'NONE',  ( 0.3155439721630312055, -0.5465381918084659674, -0.7757112907044145800 ) ) ;
#9199 = VERTEX_POINT ( 'NONE', #20945 ) ;
#9200 = AXIS2_PLACEMENT_3D ( 'NONE', #17438, #6185, #12674 ) ;
#9201 = DIRECTION ( 'NONE',  ( -7.930164461608272272E-15, -3.965082230804136136E-15, -1.000000000000000000 ) ) ;
#9202 = CARTESIAN_POINT ( 'NONE',  ( 84.99529059433409373, 176.7402077374548526, 11.00000000000001066 ) ) ;
#9203 = CARTESIAN_POINT ( 'NONE',  ( 7.342598717236928252, 0.000000000000000000, 0.000000000000000000 ) ) ;
#9204 = ORIENTED_EDGE ( 'NONE', *, *, #19625, .F. ) ;
#9205 = EDGE_CURVE ( 'NONE', #11970, #12271, #14008, .T. ) ;
#9206 = CARTESIAN_POINT ( 'NONE',  ( 229.2073078381423556, 37.71669998195577733, -16.61383192937501718 ) ) ;
#9207 = DIRECTION ( 'NONE',  ( 0.5000000000000034417, -0.8660254037844364872, 0.000000000000000000 ) ) ;
#9208 = DIRECTION ( 'NONE',  ( 0.5000000000000051070, -0.8660254037844358210, 0.000000000000000000 ) ) ;
#9209 = VERTEX_POINT ( 'NONE', #6415 ) ;
#9210 = CARTESIAN_POINT ( 'NONE',  ( 79.76867896048986495, 125.7929646387041771, 41.00000000000001421 ) ) ;
#9211 = CARTESIAN_POINT ( 'NONE',  ( 215.8239785704504072, 15.89973041162422440, -14.39661757960083222 ) ) ;
#9212 = CARTESIAN_POINT ( 'NONE',  ( 226.7034097767528067, 42.05357864125575418, -16.61383192937491771 ) ) ;
#9213 = VERTEX_POINT ( 'NONE', #5561 ) ;
#9214 = VECTOR ( 'NONE', #1509, 1000.000000000000000 ) ;
#9215 = CARTESIAN_POINT ( 'NONE',  ( 81.82126993650646796, 64.90558118418934441, 0.5045236030688061701 ) ) ;
#9216 = AXIS2_PLACEMENT_3D ( 'NONE', #6500, #5123, #4919 ) ;
#9217 = ORIENTED_EDGE ( 'NONE', *, *, #14237, .T. ) ;
#9218 = ORIENTED_EDGE ( 'NONE', *, *, #20436, .T. ) ;
#9219 = CARTESIAN_POINT ( 'NONE',  ( -1.799176528135633335, 64.25000000000000000, 2.745993778453641010 ) ) ;
#9220 = EDGE_CURVE ( 'NONE', #8218, #3255, #8754, .T. ) ;
#9221 = CONTEXT_DEPENDENT_SHAPE_REPRESENTATION ( #7566, #5497 ) ;
#9222 = DIRECTION ( 'NONE',  ( 0.4758887346169484722, 0.2747544890354094993, 0.8354878114129318245 ) ) ;
#9223 = ORIENTED_EDGE ( 'NONE', *, *, #19471, .F. ) ;
#9224 = DIRECTION ( 'NONE',  ( 0.000000000000000000, 0.000000000000000000, -1.000000000000000000 ) ) ;
#9225 = DIRECTION ( 'NONE',  ( 0.3878556453522103986, -0.6717856837524469604, -0.6310879443260485333 ) ) ;
#9226 = AXIS2_PLACEMENT_3D ( 'NONE', #1353, #17571, #12907 ) ;
#9227 = FACE_OUTER_BOUND ( 'NONE', #9337, .T. ) ;
#9228 = DIRECTION ( 'NONE',  ( -0.8660254037844357100, -0.5000000000000049960, 0.000000000000000000 ) ) ;
#9229 = EDGE_CURVE ( 'NONE', #5484, #7189, #11839, .T. ) ;
#9230 = ADVANCED_FACE ( 'NONE', ( #15252 ), #5348, .F. ) ;
#9231 = CARTESIAN_POINT ( 'NONE',  ( 218.6961259033436988, 38.05395589839552173, -11.55788255683058807 ) ) ;
#9232 = DIRECTION ( 'NONE',  ( 0.8660254037844352659, 0.5000000000000056621, 0.000000000000000000 ) ) ;
#9233 = CARTESIAN_POINT ( 'NONE',  ( 226.4334762588359524, 42.52111720895345570, -11.55788255683058807 ) ) ;
#9234 = DIRECTION ( 'NONE',  ( 0.8660254037844368202, 0.5000000000000032196, 0.000000000000000000 ) ) ;
#9235 = EDGE_LOOP ( 'NONE', ( #13280, #16164, #18602, #2547 ) ) ;
#9236 = CARTESIAN_POINT ( 'NONE',  ( 37.85427444295662269, 178.3908428320656299, 11.00000000000001243 ) ) ;
#9237 = DIRECTION ( 'NONE',  ( 0.8660254037844380415, 0.5000000000000014433, 0.000000000000000000 ) ) ;
#9238 = EDGE_CURVE ( 'NONE', #3756, #7280, #8652, .T. ) ;
#9239 = CARTESIAN_POINT ( 'NONE',  ( -15.99999999999999289, 20.09941697557067997, 4.999999999999989342 ) ) ;
#9240 = CARTESIAN_POINT ( 'NONE',  ( 200.1387714463639895, 22.66922023976253797, -14.00000000000005507 ) ) ;
#9241 = AXIS2_PLACEMENT_3D ( 'NONE', #79, #8422, #13013 ) ;
#9243 = VERTEX_POINT ( 'NONE', #2401 ) ;
#9242 = ORIENTED_EDGE ( 'NONE', *, *, #490, .F. ) ;
#9244 = FACE_OUTER_BOUND ( 'NONE', #10737, .T. ) ;
#9245 = CARTESIAN_POINT ( 'NONE',  ( -15.99999999999999289, 65.74999999999998579, 0.000000000000000000 ) ) ;
#9246 = VERTEX_POINT ( 'NONE', #6948 ) ;
#9247 = EDGE_CURVE ( 'NONE', #17344, #8219, #6383, .T. ) ;
#9248 = DIRECTION ( 'NONE',  ( 0.8528685319524385022, 0.4924038765061083955, -0.1736481776669413224 ) ) ;
#9249 = DIRECTION ( 'NONE',  ( 0.8660254037844361541, 0.5000000000000043299, 0.000000000000000000 ) ) ;
#9250 = EDGE_LOOP ( 'NONE', ( #5877, #17918, #2456, #14728 ) ) ;
#9251 = EDGE_CURVE ( 'NONE', #112, #3900, #707, .T. ) ;
#9252 = CARTESIAN_POINT ( 'NONE',  ( 201.5219881633594525, 7.288445818786272845, -2.697891510991471176 ) ) ;
#9253 = AXIS2_PLACEMENT_3D ( 'NONE', #17512, #9322, #14244 ) ;
#9254 = AXIS2_PLACEMENT_3D ( 'NONE', #2561, #9006, #6031 ) ;
#9255 = SHAPE_REPRESENTATION_RELATIONSHIP ( 'NONE' , 'NONE' ,  #6230, #3759 ) ;
#9256 = EDGE_CURVE ( 'NONE', #3379, #16821, #7161, .T. ) ;
#9257 = VERTEX_POINT ( 'NONE', #15360 ) ;
#9258 = DIRECTION ( 'NONE',  ( 0.000000000000000000, -1.000000000000000000, 0.000000000000000000 ) ) ;
#9259 = DIRECTION ( 'NONE',  ( 0.5000000000000054401, -0.8660254037844354880, 0.000000000000000000 ) ) ;
#9260 = EDGE_CURVE ( 'NONE', #2221, #16454, #3739, .T. ) ;
#9261 = DIRECTION ( 'NONE',  ( 0.000000000000000000, -0.5000000000000008882, -0.8660254037844380415 ) ) ;
#9262 = CARTESIAN_POINT ( 'NONE',  ( 214.9645700193949267, 8.238142410745643573, -4.273921076953424603 ) ) ;
#9263 = EDGE_CURVE ( 'NONE', #15282, #2193, #1602, .T. ) ;
#9264 = ORIENTED_EDGE ( 'NONE', *, *, #14603, .F. ) ;
#9265 = DIRECTION ( 'NONE',  ( 1.000000000000000000, 0.000000000000000000, 0.000000000000000000 ) ) ;
#9266 = VERTEX_POINT ( 'NONE', #18299 ) ;
#9267 = B_SPLINE_CURVE_WITH_KNOTS ( 'NONE', 3,
 ( #20117, #10665, #20525, #20321 ),
 .UNSPECIFIED., .F., .F.,
 ( 4, 4 ),
 ( 4.671652096025380568E-07, 0.0005663933874989816831 ),
 .UNSPECIFIED. ) ;
#9268 = CARTESIAN_POINT ( 'NONE',  ( -20.99999999999998224, 15.09941697557068530, 11.45643923738960446 ) ) ;
#9269 = LINE ( 'NONE', #4411, #3102 ) ;
#9270 = DIRECTION ( 'NONE',  ( -0.8660254037844354880, -0.5000000000000055511, 0.000000000000000000 ) ) ;
#9271 = VECTOR ( 'NONE', #17880, 999.9999999999998863 ) ;
#9272 = ADVANCED_FACE ( 'NONE', ( #10332 ), #13539, .T. ) ;
#9273 = DIRECTION ( 'NONE',  ( 0.03412120668232736242, -0.05909966358935653946, 0.9976687691905398170 ) ) ;
#9274 = FILL_AREA_STYLE_COLOUR ( '', #11101 ) ;
#9275 = ORIENTED_EDGE ( 'NONE', *, *, #3179, .F. ) ;
#9276 = PLANE ( 'NONE',  #14559 ) ;
#9277 = EDGE_CURVE ( 'NONE', #19534, #19903, #3774, .T. ) ;
#9278 = SURFACE_STYLE_FILL_AREA ( #15878 ) ;
#9279 = CARTESIAN_POINT ( 'NONE',  ( -16.69844302412945325, 45.63488619083994990, -12.49945479904454437 ) ) ;
#9280 = CARTESIAN_POINT ( 'NONE',  ( 105.1989074543211728, 189.2062061502930135, 11.00000000000001066 ) ) ;
#9281 = CONICAL_SURFACE ( 'NONE', #13034, 10.85470691220533190, 0.8171114040043576665 ) ;
#9282 = EDGE_CURVE ( 'NONE', #2016, #18964, #15151, .T. ) ;
#9283 = DIRECTION ( 'NONE',  ( -0.5000000000000049960, 0.8660254037844358210, -0.000000000000000000 ) ) ;
#9284 = DIRECTION ( 'NONE',  ( -5.666630594370344570E-17, 2.176694594656153859E-16, 1.000000000000000000 ) ) ;
#9286 = ORIENTED_EDGE ( 'NONE', *, *, #4874, .F. ) ;
#9285 = ORIENTED_EDGE ( 'NONE', *, *, #15499, .T. ) ;
#9287 = DIRECTION ( 'NONE',  ( -0.6634139481689433904, -0.3830222215594970003, -0.6427876096865293709 ) ) ;
#9288 = DIRECTION ( 'NONE',  ( 0.8660254037844355990, 0.5000000000000054401, 1.237624392856779246E-14 ) ) ;
#9289 = CARTESIAN_POINT ( 'NONE',  ( 228.3257519840818475, 38.59064037839600303, -10.42293161028226223 ) ) ;
#9290 = ORIENTED_EDGE ( 'NONE', *, *, #5357, .T. ) ;
#9291 = ORIENTED_EDGE ( 'NONE', *, *, #14081, .T. ) ;
#9292 = CARTESIAN_POINT ( 'NONE',  ( 226.1388791934747644, 43.03137429392007363, -11.78784277354601251 ) ) ;
#9293 = CARTESIAN_POINT ( 'NONE',  ( -0.9949668995500261515, 50.22606426727399054, -9.888289806186126185 ) ) ;
#9294 = CARTESIAN_POINT ( 'NONE',  ( -28.42825495836414618, 8.666880057480497612, -1.380138809628029595 ) ) ;
#9295 = EDGE_LOOP ( 'NONE', ( #19035, #14000, #606, #7144 ) ) ;
#9296 = EDGE_LOOP ( 'NONE', ( #10604, #5197, #7555, #9086 ) ) ;
#9297 = CARTESIAN_POINT ( 'NONE',  ( 184.9952905943350743, 3.535126980567765642, 0.9999999999999187317 ) ) ;
#9298 = CARTESIAN_POINT ( 'NONE',  ( 212.7427532632225962, 7.470596775315875071, -25.46066938576263894 ) ) ;
#9299 = CARTESIAN_POINT ( 'NONE',  ( 208.7495889232816353, 11.81532964447897704, -12.17435723916119272 ) ) ;
#9300 = AXIS2_PLACEMENT_3D ( 'NONE', #11798, #8283, #11591 ) ;
#9301 = LINE ( 'NONE', #14222, #15228 ) ;
#9302 = FACE_OUTER_BOUND ( 'NONE', #15864, .T. ) ;
#9303 = CARTESIAN_POINT ( 'NONE',  ( 226.7592937749846556, 41.63031564102205095, -17.05667259846715567 ) ) ;
#9305 = LINE ( 'NONE', #17177, #16844 ) ;
#9304 = B_SPLINE_CURVE_WITH_KNOTS ( 'NONE', 3,
 ( #2590, #7434, #13928, #5846 ),
 .UNSPECIFIED., .F., .F.,
 ( 4, 4 ),
 ( 4.349761613911982071E-05, 0.0008974833541226746782 ),
 .UNSPECIFIED. ) ;
#9306 = CARTESIAN_POINT ( 'NONE',  ( -20.48867580399955202, 17.32628949019004594, 11.66705517935763936 ) ) ;
#9307 = VERTEX_POINT ( 'NONE', #915 ) ;
#9308 = CYLINDRICAL_SURFACE ( 'NONE', #19206, 5.000000000000008882 ) ;
#9309 = DIRECTION ( 'NONE',  ( -0.8660254037844360431, -0.5000000000000046629, 0.000000000000000000 ) ) ;
#9310 = FACE_OUTER_BOUND ( 'NONE', #20443, .T. ) ;
#9311 = VERTEX_POINT ( 'NONE', #812 ) ;
#9312 = CLOSED_SHELL ( 'NONE', ( #19977, #2792, #17048, #6917, #3539, #1294, #19882, #3451, #15478, #9900, #8147, #4861, #15974, #227, #12939, #19386, #8196, #11338, #14224, #6037, #3369, #20679, #14846, #16211, #17411, #18085, #12677, #5605, #14569, #17971, #11358, #1907, #16959, #7431, #14492, #1535, #8349, #18845, #9348, #5065, #8379, #13752, #1795, #13047, #14754, #15415, #673, #12287, #2759, #19873, #11856, #14194, #6494, #6492, #16769, #4474, #16026, #20671, #9994, #19270, #9230, #17595, #13682, #12103, #16737, #11843, #58, #20057, #12485, #3751, #11768, #6485, #8342, #12014, #17358, #19112, #3964, #6168, #7670, #13856, #6234, #17461, #4075, #9764, #6531, #12530, #5782, #411, #15720, #14779, #13383, #1243, #11245, #3067, #13921, #10145, #12931, #9517, #18275, #18589, #15602, #18163, #9034, #14456, #9406, #11650, #19150, #6470, #11467, #14681, #20004, #16505, #4669, #19712, #16407, #7068, #4517, #14964, #12669, #447, #12158, #3783, #199, #3713, #10991 ) ) ;
#9313 = CARTESIAN_POINT ( 'NONE',  ( 81.31380233296179938, 64.67425244115396765, 0.4979624178218136077 ) ) ;
#9314 = EDGE_LOOP ( 'NONE', ( #6036, #15987, #6790, #5691 ) ) ;
#9315 = VECTOR ( 'NONE', #8689, 1000.000000000000114 ) ;
#9316 = ORIENTED_EDGE ( 'NONE', *, *, #8969, .T. ) ;
#9317 = CARTESIAN_POINT ( 'NONE',  ( -3.876681006550094288, 75.90505089109430514, 3.056606027154308514 ) ) ;
#9318 = VECTOR ( 'NONE', #18133, 1000.000000000000227 ) ;
#9319 = ADVANCED_FACE ( 'NONE', ( #16919 ), #5436, .T. ) ;
#9320 = SHAPE_DEFINITION_REPRESENTATION ( #17040, #1796 ) ;
#9321 =( BOUNDED_CURVE ( )  B_SPLINE_CURVE ( 3, ( #16364, #6375, #9567, #14376 ),
 .UNSPECIFIED., .F., .F. ) 
 B_SPLINE_CURVE_WITH_KNOTS ( ( 4, 4 ),
 ( 1.570796326794896558, 3.141592653589790451 ),
 .UNSPECIFIED. ) 
 CURVE ( )  GEOMETRIC_REPRESENTATION_ITEM ( )  RATIONAL_B_SPLINE_CURVE ( ( 1.000000000000000000, 0.8047378541243654926, 0.8047378541243654926, 1.000000000000000000 ) ) 
 REPRESENTATION_ITEM ( '' )  );
#9322 = DIRECTION ( 'NONE',  ( 0.5000000000000046629, -0.8660254037844360431, -4.006172263299081054E-16 ) ) ;
#9323 = EDGE_LOOP ( 'NONE', ( #9728, #16716 ) ) ;
#9324 = AXIS2_PLACEMENT_3D ( 'NONE', #12793, #19253, #11399 ) ;
#9325 = CARTESIAN_POINT ( 'NONE',  ( 225.8436831436158343, 42.88970971796653231, -12.94088743653085771 ) ) ;
#9326 = CARTESIAN_POINT ( 'NONE',  ( 59.50490953756747103, 190.8908428320656867, 11.00000000000001066 ) ) ;
#9327 = CARTESIAN_POINT ( 'NONE',  ( 197.6726886235968834, -1.230109101077226486, -14.00000000000005507 ) ) ;
#9328 = AXIS2_PLACEMENT_3D ( 'NONE', #19594, #19398, #314 ) ;
#9329 = ORIENTED_EDGE ( 'NONE', *, *, #699, .F. ) ;
#9330 = CARTESIAN_POINT ( 'NONE',  ( 62.09798184194390558, 82.78955810596320930, -19.07905325425590704 ) ) ;
#9331 = DIRECTION ( 'NONE',  ( 0.5000000000000007772, -0.8660254037844381525, 0.000000000000000000 ) ) ;
#9332 = VECTOR ( 'NONE', #14855, 1000.000000000000114 ) ;
#9333 = ADVANCED_FACE ( 'NONE', ( #2301 ), #12054, .F. ) ;
#9334 = CARTESIAN_POINT ( 'NONE',  ( 10.49211908931699178, -10.00000000000000000, 0.000000000000000000 ) ) ;
#9335 = CARTESIAN_POINT ( 'NONE',  ( 197.5592321514251353, 4.823524888127141530, -22.03054070023847544 ) ) ;
#9336 = CARTESIAN_POINT ( 'NONE',  ( 218.8611921042119093, 35.63669809411136669, -18.16400186620061064 ) ) ;
#9337 = EDGE_LOOP ( 'NONE', ( #16565, #7389, #20220, #9599, #3846, #9773, #7970, #9053 ) ) ;
#9338 = CARTESIAN_POINT ( 'NONE',  ( 32.36389338619004263, 157.9004617752989930, 4.000000000000000000 ) ) ;
#9339 = DIRECTION ( 'NONE',  ( -0.8660254037844361541, -0.5000000000000042188, 6.872020471724001723E-17 ) ) ;
#9340 = DIRECTION ( 'NONE',  ( 0.5000000000000007772, -0.8660254037844381525, 0.000000000000000000 ) ) ;
#9341 = VECTOR ( 'NONE', #8279, 1000.000000000000227 ) ;
#9342 = CARTESIAN_POINT ( 'NONE',  ( 220.2751894220140230, 35.11295958970998043, -10.21862775258423461 ) ) ;
#9343 = CARTESIAN_POINT ( 'NONE',  ( 195.2585560139913810, 8.150276080056761074, -20.52105855319921446 ) ) ;
#9344 = ADVANCED_FACE ( 'NONE', ( #4201, #10647 ), #15046, .T. ) ;
#9346 = ORIENTED_EDGE ( 'NONE', *, *, #15861, .F. ) ;
#9345 = VERTEX_POINT ( 'NONE', #12473 ) ;
#9347 = AXIS2_PLACEMENT_3D ( 'NONE', #10762, #15676, #1141 ) ;
#9348 = ADVANCED_FACE ( 'NONE', ( #20613 ), #15973, .F. ) ;
#9349 = CARTESIAN_POINT ( 'NONE',  ( 197.0236180130380319, 5.045337182940025755, -7.515250618841284869 ) ) ;
#9350 = PRESENTATION_STYLE_ASSIGNMENT (( #4498 ) ) ;
#9351 = UNCERTAINTY_MEASURE_WITH_UNIT (LENGTH_MEASURE( 1.000000000000000082E-05 ), #8932, 'distance_accuracy_value', 'NONE');
#9352 = DIRECTION ( 'NONE',  ( -1.000000000000000000, 0.000000000000000000, 0.000000000000000000 ) ) ;
#9353 = DIRECTION ( 'NONE',  ( 0.000000000000000000, 0.000000000000000000, 1.000000000000000000 ) ) ;
#9354 = CARTESIAN_POINT ( 'NONE',  ( 200.8534188064670900, 11.38047161937165974, -2.669358488461094137 ) ) ;
#9355 = EDGE_LOOP ( 'NONE', ( #6029, #847, #5662, #4091 ) ) ;
#9356 = CARTESIAN_POINT ( 'NONE',  ( 208.0983737146324870, 5.661548828456886895, -14.00000000000005507 ) ) ;
#9357 = CARTESIAN_POINT ( 'NONE',  ( 0.000000000000000000, 0.000000000000000000, 0.000000000000000000 ) ) ;
#9358 = ORIENTED_EDGE ( 'NONE', *, *, #13560, .F. ) ;
#9359 = DIRECTION ( 'NONE',  ( 0.000000000000000000, -1.000000000000000000, 0.000000000000000000 ) ) ;
#9360 = PRODUCT_RELATED_PRODUCT_CATEGORY ( 'part', '', ( #783 ) ) ;
#9361 = AXIS2_PLACEMENT_3D ( 'NONE', #6982, #2017, #8578 ) ;
#9362 = CARTESIAN_POINT ( 'NONE',  ( 62.36389338619030553, 105.9389375482328006, -12.50000000000000000 ) ) ;
#9363 = ADVANCED_FACE ( 'NONE', ( #14391 ), #15564, .T. ) ;
#9364 = DIRECTION ( 'NONE',  ( -0.5000000000000049960, 0.8660254037844357100, -0.000000000000000000 ) ) ;
#9365 = DIRECTION ( 'NONE',  ( 0.5000000000000044409, -0.8660254037844360431, -4.006172263299080068E-16 ) ) ;
#9366 = ORIENTED_EDGE ( 'NONE', *, *, #4968, .T. ) ;
#9367 = DIRECTION ( 'NONE',  ( 0.000000000000000000, 0.000000000000000000, -1.000000000000000000 ) ) ;
#9368 = EDGE_CURVE ( 'NONE', #8882, #20103, #20409, .T. ) ;
#9369 = ORIENTED_EDGE ( 'NONE', *, *, #8911, .F. ) ;
#9370 = VERTEX_POINT ( 'NONE', #1023 ) ;
#9371 = CARTESIAN_POINT ( 'NONE',  ( 228.7053588074475670, 38.58610120592910420, -14.00000000000005507 ) ) ;
#9372 = CARTESIAN_POINT ( 'NONE',  ( 207.4970939194043922, 10.91519141264829429, -2.035916199211812216 ) ) ;
#9373 = CARTESIAN_POINT ( 'NONE',  ( 184.9952905943350459, 3.535126980567737665, -6.000000000000071942 ) ) ;
#9374 = EDGE_CURVE ( 'NONE', #2644, #19458, #17448, .T. ) ;
#9375 = CARTESIAN_POINT ( 'NONE',  ( 80.00000000000000000, 4.819735792371784729E-16, -4.172000000000029907 ) ) ;
#9376 = CARTESIAN_POINT ( 'NONE',  ( 214.6606502076888034, 14.87405588687143698, -20.76014333877609275 ) ) ;
#9377 = ORIENTED_EDGE ( 'NONE', *, *, #11443, .T. ) ;
#9378 = EDGE_CURVE ( 'NONE', #17095, #2754, #3027, .T. ) ;
#9379 = CARTESIAN_POINT ( 'NONE',  ( 220.0968443491207722, 35.00999201386641602, -10.43865930680574827 ) ) ;
#9380 = ORIENTED_EDGE ( 'NONE', *, *, #5508, .F. ) ;
#9381 =( NAMED_UNIT ( * ) PLANE_ANGLE_UNIT ( ) SI_UNIT ( $, .RADIAN. ) );
#9382 = CARTESIAN_POINT ( 'NONE',  ( -7.293433234389345543, 44.99741180067891122, -8.975862722551676498 ) ) ;
#9383 = DIRECTION ( 'NONE',  ( -1.060575238724903217E-16, -6.123233995736827666E-17, 1.000000000000000000 ) ) ;
#9384 = EDGE_CURVE ( 'NONE', #16336, #7423, #10866, .T. ) ;
#9385 = CARTESIAN_POINT ( 'NONE',  ( 215.0759710110270646, 15.29085814165182455, -19.44895743303496261 ) ) ;
#9386 = CARTESIAN_POINT ( 'NONE',  ( -21.92567948885827178, 45.20990627917875315, -11.03350026938877093 ) ) ;
#9387 = VECTOR ( 'NONE', #17978, 1000.000000000000227 ) ;
#9389 = ORIENTED_EDGE ( 'NONE', *, *, #2493, .F. ) ;
#9388 = ORIENTED_EDGE ( 'NONE', *, *, #7327, .T. ) ;
#9390 = CARTESIAN_POINT ( 'NONE',  ( 219.8530131173444033, 35.43232009577518227, -17.56803216753788988 ) ) ;
#9391 = CARTESIAN_POINT ( 'NONE',  ( 230.0621173633032299, 36.23612645358366535, -14.58164069303002819 ) ) ;
#9392 = CIRCLE ( 'NONE', #8044, 3.619616396367202782 ) ;
#9393 = CARTESIAN_POINT ( 'NONE',  ( 1.469533291826635724, 76.75544209469038037, -3.174647668802506484 ) ) ;
#9394 = ORIENTED_EDGE ( 'NONE', *, *, #14243, .T. ) ;
#9395 = ORIENTED_EDGE ( 'NONE', *, *, #17337, .T. ) ;
#9396 = VERTEX_POINT ( 'NONE', #2927 ) ;
#9397 = CARTESIAN_POINT ( 'NONE',  ( -15.99999999999999289, 80.00000000000000000, 0.000000000000000000 ) ) ;
#9398 = CARTESIAN_POINT ( 'NONE',  ( 198.6336827526812669, -1.448098972604089374, -15.39542905462715261 ) ) ;
#9399 = CARTESIAN_POINT ( 'NONE',  ( -19.92414059662587533, 50.39646155737152355, -15.92985716015406972 ) ) ;
#9400 = EDGE_CURVE ( 'NONE', #18781, #3452, #13260, .T. ) ;
#9401 = CARTESIAN_POINT ( 'NONE',  ( 207.1242269781990331, 15.00092440535764560, -26.58724934764018855 ) ) ;
#9402 = EDGE_CURVE ( 'NONE', #20090, #17792, #2722, .T. ) ;
#9403 = EDGE_LOOP ( 'NONE', ( #426, #3800, #10578, #10403 ) ) ;
#9404 = ORIENTED_EDGE ( 'NONE', *, *, #11984, .T. ) ;
#9405 = DIRECTION ( 'NONE',  ( -0.5000000000000008882, 0.8660254037844381525, 0.000000000000000000 ) ) ;
#9406 = ADVANCED_FACE ( 'NONE', ( #12373 ), #8495, .T. ) ;
#9407 =( LENGTH_UNIT ( ) NAMED_UNIT ( * ) SI_UNIT ( .MILLI., .METRE. ) );
#9408 = DIRECTION ( 'NONE',  ( -0.5000000000000049960, 0.8660254037844358210, -0.000000000000000000 ) ) ;
#9409 = VECTOR ( 'NONE', #10894, 1000.000000000000114 ) ;
#9410 = CARTESIAN_POINT ( 'NONE',  ( -11.00000000000000355, 15.09941697557068530, 11.45643923738960446 ) ) ;
#9411 = DIRECTION ( 'NONE',  ( -1.000000000000000000, -0.000000000000000000, -0.000000000000000000 ) ) ;
#9412 = AXIS2_PLACEMENT_3D ( 'NONE', #16875, #12105, #2252 ) ;
#9413 = EDGE_CURVE ( 'NONE', #15824, #20638, #10874, .T. ) ;
#9414 = CARTESIAN_POINT ( 'NONE',  ( 229.7650217427808172, 36.75071116303467988, -13.95414044509044160 ) ) ;
#9415 = CARTESIAN_POINT ( 'NONE',  ( -27.42006910542679776, 68.94695149080686747, 5.083831496961733976 ) ) ;
#9416 = PLANE ( 'NONE',  #16693 ) ;
#9417 = ADVANCED_FACE ( 'NONE', ( #7578, #1233, #14070, #14180, #10980 ), #18931, .T. ) ;
#9418 = DIRECTION ( 'NONE',  ( 1.000000000000000000, 0.000000000000000000, 0.000000000000000000 ) ) ;
#9419 = CARTESIAN_POINT ( 'NONE',  ( 206.8794782033451156, 3.312613250519402808, -26.96550585544242296 ) ) ;
#9420 = FACE_OUTER_BOUND ( 'NONE', #5869, .T. ) ;
#9421 = ORIENTED_EDGE ( 'NONE', *, *, #3422, .T. ) ;
#9422 = CARTESIAN_POINT ( 'NONE',  ( 67.37294370578848657, 72.35496154219596576, -1.763419216299827008 ) ) ;
#9423 = EDGE_LOOP ( 'NONE', ( #7601, #12493, #3924, #17650, #11103, #3028 ) ) ;
#9424 = VECTOR ( 'NONE', #10938, 1000.000000000000114 ) ;
#9425 = VERTEX_POINT ( 'NONE', #15863 ) ;
#9426 = CARTESIAN_POINT ( 'NONE',  ( 0.6802973005055915623, 71.85025536417184355, 0.8468720397213821416 ) ) ;
#9427 = ADVANCED_FACE ( 'NONE', ( #1336 ), #20508, .F. ) ;
#9428 = CARTESIAN_POINT ( 'NONE',  ( -20.63965592820711237, 79.99566203514093843, -12.08264426539709468 ) ) ;
#9429 = B_SPLINE_CURVE_WITH_KNOTS ( 'NONE', 3,
 ( #14095, #3154, #7706, #12602 ),
 .UNSPECIFIED., .F., .F.,
 ( 4, 4 ),
 ( 7.698220069962578513E-05, 0.0007496329927527359965 ),
 .UNSPECIFIED. ) ;
#9430 = DIRECTION ( 'NONE',  ( 0.000000000000000000, 6.938893903907177533E-18, 1.000000000000000000 ) ) ;
#9431 = ORIENTED_EDGE ( 'NONE', *, *, #6141, .T. ) ;
#9432 = LINE ( 'NONE', #1502, #5005 ) ;
#9433 = DIRECTION ( 'NONE',  ( 0.000000000000000000, -0.000000000000000000, 1.000000000000000000 ) ) ;
#9434 = FACE_OUTER_BOUND ( 'NONE', #2375, .T. ) ;
#9435 = CYLINDRICAL_SURFACE ( 'NONE', #6102, 12.47473710546057646 ) ;
#9436 = AXIS2_PLACEMENT_3D ( 'NONE', #11774, #640, #14767 ) ;
#9437 = LINE ( 'NONE', #1407, #6603 ) ;
#9438 = CARTESIAN_POINT ( 'NONE',  ( 199.2243387870319395, 21.03182819120163671, -14.00000000000005507 ) ) ;
#9439 = CARTESIAN_POINT ( 'NONE',  ( 226.8193494925532150, 41.85276516287428450, -10.82724490084729929 ) ) ;
#9440 = CARTESIAN_POINT ( 'NONE',  ( 190.9298951392057120, 16.26579628913994213, -5.993340328401665751 ) ) ;
#9441 = ADVANCED_FACE ( 'NONE', ( #5981, #11080 ), #6083, .T. ) ;
#9442 = CARTESIAN_POINT ( 'NONE',  ( 229.4605141275517894, 37.27813382390270647, -16.48323849494068227 ) ) ;
#9443 = EDGE_LOOP ( 'NONE', ( #19381, #6303, #810, #3517 ) ) ;
#9444 = CARTESIAN_POINT ( 'NONE',  ( 218.4477085251713504, 9.991534140873421066, -9.972943347742013742 ) ) ;
#9445 = CARTESIAN_POINT ( 'NONE',  ( 59.12602517596783969, 85.07731064195019144, -9.828416369996476831 ) ) ;
#9446 = DIRECTION ( 'NONE',  ( 0.000000000000000000, 0.000000000000000000, -1.000000000000000000 ) ) ;
#9447 = LINE ( 'NONE', #35, #5019 ) ;
#9448 = CIRCLE ( 'NONE', #19288, 3.999999999999999112 ) ;
#9450 = ORIENTED_EDGE ( 'NONE', *, *, #4975, .F. ) ;
#9449 = ORIENTED_EDGE ( 'NONE', *, *, #6861, .F. ) ;
#9451 = VERTEX_POINT ( 'NONE', #17664 ) ;
#9452 = AXIS2_PLACEMENT_3D ( 'NONE', #17149, #15681, #12065 ) ;
#9453 = SURFACE_STYLE_USAGE ( .BOTH. , #4695 ) ;
#9454 = AXIS2_PLACEMENT_3D ( 'NONE', #4532, #12804, #4733 ) ;
#9455 = CARTESIAN_POINT ( 'NONE',  ( 221.7170026686113147, 32.20379548820332616, -14.53509620734056540 ) ) ;
#9456 = ORIENTED_EDGE ( 'NONE', *, *, #15898, .F. ) ;
#9457 = EDGE_CURVE ( 'NONE', #15788, #2452, #6792, .T. ) ;
#9458 = CARTESIAN_POINT ( 'NONE',  ( -30.58332872481887321, 79.14063577707173636, -7.486051927416412788 ) ) ;
#9459 = FACE_OUTER_BOUND ( 'NONE', #823, .T. ) ;
#9460 = VECTOR ( 'NONE', #11898, 1000.000000000000227 ) ;
#9461 = CARTESIAN_POINT ( 'NONE',  ( 190.7433706042750146, 35.72129598111152404, -19.00000000000003908 ) ) ;
#9462 = ORIENTED_EDGE ( 'NONE', *, *, #12642, .T. ) ;
#9463 = CARTESIAN_POINT ( 'NONE',  ( 200.1605181682011221, -0.5665801344454006738, -7.448751785191272567 ) ) ;
#9464 = ADVANCED_FACE ( 'NONE', ( #16269 ), #11394, .F. ) ;
#9465 = CARTESIAN_POINT ( 'NONE',  ( 221.2084640702248635, 33.49648048159280478, -17.11800046810217779 ) ) ;
#9466 = AXIS2_PLACEMENT_3D ( 'NONE', #18483, #3955, #10404 ) ;
#9467 = CARTESIAN_POINT ( 'NONE',  ( 203.9637611243273057, 8.521181414665040421, -26.28791492288515386 ) ) ;
#9468 = CARTESIAN_POINT ( 'NONE',  ( 199.3642739955437833, 5.865666282727633352, -4.003039906353938804 ) ) ;
#9469 = CIRCLE ( 'NONE', #19640, 2.499999999999997780 ) ;
#9470 = VERTEX_POINT ( 'NONE', #1854 ) ;
#9471 = CARTESIAN_POINT ( 'NONE',  ( 226.6211368133091923, 39.11482588413117867, -14.00000000000005507 ) ) ;
#9472 = ORIENTED_EDGE ( 'NONE', *, *, #4604, .F. ) ;
#9473 = DIRECTION ( 'NONE',  ( -0.8660254037844355990, -0.5000000000000055511, 0.000000000000000000 ) ) ;
#9474 = CARTESIAN_POINT ( 'NONE',  ( -35.00000000000000000, 64.25000000000000000, 75.00000000000000000 ) ) ;
#9475 = FACE_OUTER_BOUND ( 'NONE', #7100, .T. ) ;
#9476 = AXIS2_PLACEMENT_3D ( 'NONE', #8950, #3101, #14061 ) ;
#9477 = ADVANCED_FACE ( 'NONE', ( #372 ), #16474, .T. ) ;
#9478 = DIRECTION ( 'NONE',  ( -0.000000000000000000, 1.000000000000000000, -0.000000000000000000 ) ) ;
#9479 = LINE ( 'NONE', #4524, #20568 ) ;
#9480 =( GEOMETRIC_REPRESENTATION_CONTEXT ( 3 ) GLOBAL_UNCERTAINTY_ASSIGNED_CONTEXT ( ( #9351 ) ) GLOBAL_UNIT_ASSIGNED_CONTEXT ( ( #8932, #571, #12122 ) ) REPRESENTATION_CONTEXT ( 'NONE', 'WORKASPACE' ) );
#9481 = ORIENTED_EDGE ( 'NONE', *, *, #9109, .T. ) ;
#9482 = VECTOR ( 'NONE', #15692, 1000.000000000000000 ) ;
#9483 = CARTESIAN_POINT ( 'NONE',  ( 219.8878554188805481, 35.34223952461786666, -10.43865930680574827 ) ) ;
#9484 = VECTOR ( 'NONE', #17583, 1000.000000000000114 ) ;
#9485 = EDGE_CURVE ( 'NONE', #1053, #6174, #14704, .T. ) ;
#9486 = EDGE_LOOP ( 'NONE', ( #8647, #13117, #8124 ) ) ;
#9487 = EDGE_CURVE ( 'NONE', #12506, #884, #14491, .T. ) ;
#9488 = CARTESIAN_POINT ( 'NONE',  ( 215.0768188481721381, 15.46835754483921832, -19.61062504997882172 ) ) ;
#9489 = CARTESIAN_POINT ( 'NONE',  ( -5.931730174668158106, 45.09262939792821356, -7.439426869663584796 ) ) ;
#9490 = DIRECTION ( 'NONE',  ( -0.5000000000000027756, 0.8660254037844372643, -0.000000000000000000 ) ) ;
#9491 = AXIS2_PLACEMENT_3D ( 'NONE', #15508, #6138, #20353 ) ;
#9492 = CARTESIAN_POINT ( 'NONE',  ( 173.9132435853527454, 54.87193107572242212, -14.00000000000002842 ) ) ;
#9493 = AXIS2_PLACEMENT_3D ( 'NONE', #4267, #7541, #14033 ) ;
#9494 = CARTESIAN_POINT ( 'NONE',  ( -20.16417779879374450, 45.40494962656599398, -11.79224875690949759 ) ) ;
#9496 = VERTEX_POINT ( 'NONE', #17871 ) ;
#9495 = VERTEX_POINT ( 'NONE', #20918 ) ;
#9497 = AXIS2_PLACEMENT_3D ( 'NONE', #3466, #1672, #20840 ) ;
#9498 = ORIENTED_EDGE ( 'NONE', *, *, #20128, .T. ) ;
#9499 = CARTESIAN_POINT ( 'NONE',  ( 218.4113082942438666, 37.92942609890246786, -15.81459191843834944 ) ) ;
#9500 = CARTESIAN_POINT ( 'NONE',  ( 197.7441788599589074, -1.188834193869147571, -15.43274561385865873 ) ) ;
#9501 = CARTESIAN_POINT ( 'NONE',  ( -10.87002103192357616, 79.99099046118973888, -11.97147087691752532 ) ) ;
#9502 = AXIS2_PLACEMENT_3D ( 'NONE', #57, #9981, #1957 ) ;
#9503 = ORIENTED_EDGE ( 'NONE', *, *, #5834, .T. ) ;
#9504 = VERTEX_POINT ( 'NONE', #9783 ) ;
#9505 = EDGE_CURVE ( 'NONE', #11970, #9246, #9580, .T. ) ;
#9506 = ORIENTED_EDGE ( 'NONE', *, *, #11620, .F. ) ;
#9507 = CARTESIAN_POINT ( 'NONE',  ( 54.01452848080093361, 170.4004617752990498, 4.000000000000000000 ) ) ;
#9508 = CARTESIAN_POINT ( 'NONE',  ( 195.2241281744312857, 3.829391336032939908, -15.41371838794996840 ) ) ;
#9509 = CARTESIAN_POINT ( 'NONE',  ( 218.5578050973448683, 38.29353456212945872, -11.94979443502191074 ) ) ;
#9510 = CARTESIAN_POINT ( 'NONE',  ( 208.8107687779841228, 4.427644383670616079, -14.00000000000005507 ) ) ;
#9511 = EDGE_LOOP ( 'NONE', ( #12077, #12532, #1996, #19273 ) ) ;
#9512 = ORIENTED_EDGE ( 'NONE', *, *, #4715, .F. ) ;
#9513 = LINE ( 'NONE', #14422, #9035 ) ;
#9514 = EDGE_CURVE ( 'NONE', #16498, #13841, #18661, .T. ) ;
#9515 = AXIS2_PLACEMENT_3D ( 'NONE', #63, #4824, #1447 ) ;
#9516 = PLANE ( 'NONE',  #11813 ) ;
#9517 = ADVANCED_FACE ( 'NONE', ( #8194 ), #8297, .T. ) ;
#9518 = AXIS2_PLACEMENT_3D ( 'NONE', #7517, #17278, #14120 ) ;
#9519 = DIRECTION ( 'NONE',  ( 0.8660254037844370423, 0.5000000000000026645, -0.000000000000000000 ) ) ;
#9520 = CARTESIAN_POINT ( 'NONE',  ( -28.72613570046926768, 61.69439188727080392, 2.139313856061467511 ) ) ;
#9521 = LINE ( 'NONE', #4864, #7209 ) ;
#9522 = AXIS2_PLACEMENT_3D ( 'NONE', #2919, #14171, #20607 ) ;
#9523 = DIRECTION ( 'NONE',  ( 0.000000000000000000, 0.000000000000000000, -1.000000000000000000 ) ) ;
#9524 = LINE ( 'NONE', #11337, #138 ) ;
#9525 = FACE_OUTER_BOUND ( 'NONE', #893, .T. ) ;
#9526 = ORIENTED_EDGE ( 'NONE', *, *, #18549, .F. ) ;
#9527 = CARTESIAN_POINT ( 'NONE',  ( 82.79352064649921772, 63.77227335278520570, 0.5678441448316937645 ) ) ;
#9528 = EDGE_CURVE ( 'NONE', #14678, #12709, #18326, .T. ) ;
#9529 = ORIENTED_EDGE ( 'NONE', *, *, #307, .F. ) ;
#9530 = ADVANCED_FACE ( 'NONE', ( #4819 ), #731, .F. ) ;
#9531 = ORIENTED_EDGE ( 'NONE', *, *, #3208, .T. ) ;
#9532 = CARTESIAN_POINT ( 'NONE',  ( 229.8901273022082421, 36.53402197779678318, -13.49489896056993743 ) ) ;
#9533 = DIRECTION ( 'NONE',  ( 0.000000000000000000, 0.000000000000000000, 1.000000000000000000 ) ) ;
#9534 = AXIS2_PLACEMENT_3D ( 'NONE', #48, #6488, #11384 ) ;
#9535 = VECTOR ( 'NONE', #20382, 1000.000000000000114 ) ;
#9536 = CARTESIAN_POINT ( 'NONE',  ( -29.92243289137827134, 79.32232495077528256, -8.031676520616485959 ) ) ;
#9537 = SHAPE_DEFINITION_REPRESENTATION ( #15013, #20602 ) ;
#9538 = VECTOR ( 'NONE', #18480, 1000.000000000000227 ) ;
#9539 = EDGE_CURVE ( 'NONE', #19576, #12179, #16078, .T. ) ;
#9540 = CARTESIAN_POINT ( 'NONE',  ( 226.2091685456994981, 41.93016367357235197, -11.12998660979000931 ) ) ;
#9541 = ORIENTED_EDGE ( 'NONE', *, *, #17600, .T. ) ;
#9542 = FACE_OUTER_BOUND ( 'NONE', #8095, .T. ) ;
#9543 = DIRECTION ( 'NONE',  ( 1.000000000000000000, -0.000000000000000000, -0.000000000000000000 ) ) ;
#9544 = DIRECTION ( 'NONE',  ( 0.8660254037844360431, 0.5000000000000044409, -5.976026924694053325E-17 ) ) ;
#9545 = FACE_OUTER_BOUND ( 'NONE', #2104, .T. ) ;
#9546 = FACE_OUTER_BOUND ( 'NONE', #14624, .T. ) ;
#9547 = CARTESIAN_POINT ( 'NONE',  ( 218.1639642825640522, 38.35783849407987844, -13.95097276009430587 ) ) ;
#9548 = VECTOR ( 'NONE', #18378, 1000.000000000000114 ) ;
#9549 = EDGE_CURVE ( 'NONE', #18916, #11617, #19752, .T. ) ;
#9550 = TOROIDAL_SURFACE ( 'NONE', #1113, 6.500000000000000888, 1.500000000000000000 ) ;
#9551 = CARTESIAN_POINT ( 'NONE',  ( -11.00000000000000355, 15.09941697557068530, 11.45643923738960446 ) ) ;
#9552=STYLED_ITEM('',(#20995),#10492);
#9553 = CARTESIAN_POINT ( 'NONE',  ( 225.5964691407864677, 42.99139017264894136, -13.49489896056980420 ) ) ;
#9554 = LINE ( 'NONE', #14257, #20344 ) ;
#9555 = CARTESIAN_POINT ( 'NONE',  ( -11.59722103597593801, 18.53029315133363752, 3.430876175762952673 ) ) ;
#9556 = EDGE_LOOP ( 'NONE', ( #4428, #16176, #13374, #17947, #9242, #14046 ) ) ;
#9557 = CARTESIAN_POINT ( 'NONE',  ( 212.8960219706529813, 6.786266414165766925, -3.025685634606239294 ) ) ;
#9558 = CARTESIAN_POINT ( 'NONE',  ( 82.92989559899719154, 62.71207119171138800, 0.4539515997919767454 ) ) ;
#9559 = LINE ( 'NONE', #8958, #18620 ) ;
#9560 = FACE_OUTER_BOUND ( 'NONE', #11678, .T. ) ;
#9562 = ORIENTED_EDGE ( 'NONE', *, *, #10951, .F. ) ;
#9561 = VERTEX_POINT ( 'NONE', #6701 ) ;
#9563 = ORIENTED_EDGE ( 'NONE', *, *, #16779, .F. ) ;
#9564 = SURFACE_SIDE_STYLE ('',( #12666 ) ) ;
#9565 = PRODUCT_DEFINITION_CONTEXT ( 'detailed design', #17457, 'design' ) ;
#9566 = VECTOR ( 'NONE', #2766, 1000.000000000000227 ) ;
#9567 = CARTESIAN_POINT ( 'NONE',  ( 183.9132435853528307, 37.55142300003366529, -11.07106781186552524 ) ) ;
#9568 = ORIENTED_EDGE ( 'NONE', *, *, #16519, .F. ) ;
#9569 = DIRECTION ( 'NONE',  ( 0.4814586436739026754, -0.8339108325863923143, 0.2697967711570247729 ) ) ;
#9570 = CARTESIAN_POINT ( 'NONE',  ( -26.44938323691329884, 79.57013539180375972, -8.777265990090930003 ) ) ;
#9571 = CARTESIAN_POINT ( 'NONE',  ( 221.4549246441689263, 32.86364614288974906, -16.35636678495291818 ) ) ;
#9572 = ORIENTED_EDGE ( 'NONE', *, *, #19257, .F. ) ;
#9573 = CARTESIAN_POINT ( 'NONE',  ( 4.000000000000000000, 1.759474945355379960, -3.047500000000001652 ) ) ;
#9574 = CARTESIAN_POINT ( 'NONE',  ( 210.3388300726135753, 6.082691074106562290, -26.28791492288521425 ) ) ;
#9575 = DIRECTION ( 'NONE',  ( 0.000000000000000000, 0.000000000000000000, 1.000000000000000000 ) ) ;
#9576 = ORIENTED_EDGE ( 'NONE', *, *, #9648, .F. ) ;
#9577 = CARTESIAN_POINT ( 'NONE',  ( 5.000000000000004441, 0.000000000000000000, 0.000000000000000000 ) ) ;
#9578 = DIRECTION ( 'NONE',  ( -0.8660254037844372643, -0.5000000000000024425, 0.000000000000000000 ) ) ;
#9579 = ORIENTED_EDGE ( 'NONE', *, *, #4504, .F. ) ;
#9580 = LINE ( 'NONE', #156, #1067 ) ;
#9581 = EDGE_LOOP ( 'NONE', ( #8624, #11413, #13538, #2195 ) ) ;
#9582 = CARTESIAN_POINT ( 'NONE',  ( 211.2177619293863131, 27.70070338464699589, -12.73925315114813372 ) ) ;
#9583 = DIRECTION ( 'NONE',  ( 0.8660254037844352659, 0.5000000000000056621, 0.000000000000000000 ) ) ;
#9584 = DIRECTION ( 'NONE',  ( 0.5000000000000051070, -0.8660254037844359321, 0.000000000000000000 ) ) ;
#9585 = CARTESIAN_POINT ( 'NONE',  ( 10.49211908931699178, 5.000000000000000000, 0.000000000000000000 ) ) ;
#9586 = EDGE_CURVE ( 'NONE', #12995, #17291, #1545, .T. ) ;
#9587 = CARTESIAN_POINT ( 'NONE',  ( -30.00000000000005329, 4.999999999999980460, -7.692611737894555546 ) ) ;
#9588 = VECTOR ( 'NONE', #10483, 1000.000000000000114 ) ;
#9589 = ORIENTED_EDGE ( 'NONE', *, *, #20551, .F. ) ;
#9590 = B_SPLINE_CURVE_WITH_KNOTS ( 'NONE', 3,
 ( #2625, #17241, #2832, #10557, #1027, #20617, #18836, #19049, #9068, #18733, #20414, #10986, #5882, #12377 ),
 .UNSPECIFIED., .F., .F.,
 ( 4, 2, 2, 2, 2, 2, 4 ),
 ( 0.08478205796461193988, 0.08763025155739845307, 0.09047844515018496625, 0.09190254194657822284, 0.09332663874297149331, 0.09475073553936474990, 0.09617483233575800650 ),
 .UNSPECIFIED. ) ;
#9591 = CARTESIAN_POINT ( 'NONE',  ( 211.7320635740234422, 6.114254720546163924, -25.34310559273333396 ) ) ;
#9592 = EDGE_LOOP ( 'NONE', ( #19779, #11822, #845, #1076 ) ) ;
#9593 = CARTESIAN_POINT ( 'NONE',  ( 10.49211908931699178, -10.00000000000000000, 5.999999999999998224 ) ) ;
#9594 = CARTESIAN_POINT ( 'NONE',  ( -5.369514813894758376, 45.26689869013502232, -6.584760213112335947 ) ) ;
#9595 = DIRECTION ( 'NONE',  ( -0.8660254037844354880, -0.5000000000000055511, 0.000000000000000000 ) ) ;
#9596 = CARTESIAN_POINT ( 'NONE',  ( 93.04593889385130012, 210.2557651598135351, 11.00000000000001066 ) ) ;
#9597 = ADVANCED_FACE ( 'NONE', ( #6597 ), #1747, .T. ) ;
#9598 = CARTESIAN_POINT ( 'NONE',  ( -26.45282069710705386, 45.18437375736277062, -6.897582699900483227 ) ) ;
#9600 = VERTEX_POINT ( 'NONE', #17967 ) ;
#9599 = ORIENTED_EDGE ( 'NONE', *, *, #9858, .T. ) ;
#9601 = EDGE_LOOP ( 'NONE', ( #20913, #18205 ) ) ;
#9602 = ORIENTED_EDGE ( 'NONE', *, *, #10043, .T. ) ;
#9603 = CONICAL_SURFACE ( 'NONE', #4206, 4.389613146203297234, 1.047197551196619614 ) ;
#9604 = CARTESIAN_POINT ( 'NONE',  ( 218.9149645394843731, 10.51890375032455438, -16.79062062844375092 ) ) ;
#9605 = CARTESIAN_POINT ( 'NONE',  ( 219.6853205409617260, 35.92869035892709917, -10.38579831631091643 ) ) ;
#9606 = CARTESIAN_POINT ( 'NONE',  ( -8.197862634022071049, 79.89664383654030644, -10.58772689523680377 ) ) ;
#9607 = VERTEX_POINT ( 'NONE', #14595 ) ;
#9608 = ORIENTED_EDGE ( 'NONE', *, *, #8743, .T. ) ;
#9609 = VERTEX_POINT ( 'NONE', #12994 ) ;
#9610 = CARTESIAN_POINT ( 'NONE',  ( 226.9772257381708300, 41.25284640819057103, -10.68456754651930218 ) ) ;
#9611 = LINE ( 'NONE', #3471, #3742 ) ;
#9612 = LINE ( 'NONE', #1886, #11896 ) ;
#9613 = CARTESIAN_POINT ( 'NONE',  ( 214.1110484215691656, 14.37972046727219144, -5.993340328401894013 ) ) ;
#9614 = ORIENTED_EDGE ( 'NONE', *, *, #6796, .T. ) ;
#9615 = EDGE_CURVE ( 'NONE', #18407, #16739, #19436, .T. ) ;
#9616 = ORIENTED_EDGE ( 'NONE', *, *, #19317, .T. ) ;
#9617 = EDGE_CURVE ( 'NONE', #566, #16219, #19540, .T. ) ;
#9618 = DIRECTION ( 'NONE',  ( 0.000000000000000000, 0.4999999999999987232, -0.8660254037844393737 ) ) ;
#9619 =( NAMED_UNIT ( * ) PLANE_ANGLE_UNIT ( ) SI_UNIT ( $, .RADIAN. ) );
#9620 = VECTOR ( 'NONE', #1431, 999.9999999999998863 ) ;
#9621 = DIRECTION ( 'NONE',  ( -0.8660254037844371533, -0.5000000000000025535, 0.000000000000000000 ) ) ;
#9622 = EDGE_CURVE ( 'NONE', #18235, #17008, #2078, .T. ) ;
#9623 = CARTESIAN_POINT ( 'NONE',  ( 198.0735972701637024, -1.389238810292188875, -14.00000000000005507 ) ) ;
#9624 = CARTESIAN_POINT ( 'NONE',  ( -28.76203598978908005, 60.93597901302553055, 1.948583232574534696 ) ) ;
#9625 = CARTESIAN_POINT ( 'NONE',  ( -15.99999999999999289, 80.00000000000000000, 4.999999999999989342 ) ) ;
#9626 = EDGE_LOOP ( 'NONE', ( #16308, #20367, #12729, #6419 ) ) ;
#9627 = DIRECTION ( 'NONE',  ( 0.000000000000000000, 0.000000000000000000, 1.000000000000000000 ) ) ;
#9628 = DIRECTION ( 'NONE',  ( -0.4758887346169485832, -0.2747544890354092773, -0.8354878114129317135 ) ) ;
#9629 = FACE_OUTER_BOUND ( 'NONE', #2724, .T. ) ;
#9630 = EDGE_LOOP ( 'NONE', ( #2620, #13360, #20109, #12526, #494 ) ) ;
#9631 = VERTEX_POINT ( 'NONE', #7238 ) ;
#9633 = EDGE_CURVE ( 'NONE', #13156, #5664, #13602, .T. ) ;
#9632 = CARTESIAN_POINT ( 'NONE',  ( 54.35552982649267051, 77.95337578947557233, -11.36981949127928893 ) ) ;
#9634 = ORIENTED_EDGE ( 'NONE', *, *, #14045, .T. ) ;
#9635 = ORIENTED_EDGE ( 'NONE', *, *, #5639, .F. ) ;
#9636 = CARTESIAN_POINT ( 'NONE',  ( 0.3880700646982117585, 70.47620764902606538, 1.501429235142761609 ) ) ;
#9637 = EDGE_CURVE ( 'NONE', #5435, #15672, #8934, .T. ) ;
#9638 = SHAPE_REPRESENTATION ( 'Drill Head Clamping Component', ( #18233 ), #2676 ) ;
#9639 = AXIS2_PLACEMENT_3D ( 'NONE', #10644, #1019, #18825 ) ;
#9640 = ORIENTED_EDGE ( 'NONE', *, *, #1479, .F. ) ;
#9641 = FACE_OUTER_BOUND ( 'NONE', #17854, .T. ) ;
#9642 = DIRECTION ( 'NONE',  ( 0.8660254037844360431, 0.5000000000000045519, 4.336808689942050277E-16 ) ) ;
#9643 = ORIENTED_EDGE ( 'NONE', *, *, #13388, .T. ) ;
#9644 = EDGE_CURVE ( 'NONE', #8299, #17056, #2426, .T. ) ;
#9645 = PLANE ( 'NONE',  #16220 ) ;
#9646 = CARTESIAN_POINT ( 'NONE',  ( 209.6747333788187291, 30.08054303420691866, -16.41975067815232947 ) ) ;
#9647 = DIRECTION ( 'NONE',  ( -0.1992005449231190328, 0.3450254647022464871, -0.9172113015054553786 ) ) ;
#9648 = EDGE_CURVE ( 'NONE', #5150, #3223, #20072, .T. ) ;
#9649 = CARTESIAN_POINT ( 'NONE',  ( 221.5793113145849134, 32.44228390914006610, -15.46846178913030201 ) ) ;
#9650 = DIRECTION ( 'NONE',  ( 0.8660254037844355990, 0.5000000000000054401, 0.000000000000000000 ) ) ;
#9651 = CIRCLE ( 'NONE', #3908, 13.50000000000000711 ) ;
#9652 = CARTESIAN_POINT ( 'NONE',  ( 30.10683012259193703, 0.000000000000000000, 5.999999999999998224 ) ) ;
#9653 = PLANE ( 'NONE',  #4190 ) ;
#9654 = DIRECTION ( 'NONE',  ( 0.8660254037844370423, 0.5000000000000026645, -0.000000000000000000 ) ) ;
#9655 = AXIS2_PLACEMENT_3D ( 'NONE', #655, #11899, #2572 ) ;
#9656 = ORIENTED_EDGE ( 'NONE', *, *, #104, .T. ) ;
#9657 = AXIS2_PLACEMENT_3D ( 'NONE', #4456, #6027, #13791 ) ;
#9658 = B_SPLINE_CURVE_WITH_KNOTS ( 'NONE', 3,
 ( #16550, #2032, #1930, #8376 ),
 .UNSPECIFIED., .F., .F.,
 ( 4, 4 ),
 ( 4.692417266935620115E-07, 0.0008544549797101211232 ),
 .UNSPECIFIED. ) ;
#9660 = EDGE_CURVE ( 'NONE', #17870, #10441, #15966, .T. ) ;
#9659 = FACE_OUTER_BOUND ( 'NONE', #10142, .T. ) ;
#9661 = CARTESIAN_POINT ( 'NONE',  ( 209.3990796341988982, 4.767305814873403769, -25.92587471718750436 ) ) ;
#9662 = B_SPLINE_CURVE_WITH_KNOTS ( 'NONE', 3,
 ( #2152, #8389, #6902, #5303 ),
 .UNSPECIFIED., .F., .F.,
 ( 4, 4 ),
 ( 6.921599877329810507E-07, 0.0005666183822833390600 ),
 .UNSPECIFIED. ) ;
#9663 = CARTESIAN_POINT ( 'NONE',  ( 45.00000000000000000, 5.000000000000000000, -15.00000000000000000 ) ) ;
#9664 = FACE_OUTER_BOUND ( 'NONE', #15225, .T. ) ;
#9666 = VERTEX_POINT ( 'NONE', #476 ) ;
#9665 = VERTEX_POINT ( 'NONE', #2063 ) ;
#9667 = AXIS2_PLACEMENT_3D ( 'NONE', #1029, #7791, #7484 ) ;
#9668 = EDGE_CURVE ( 'NONE', #18332, #6104, #16306, .T. ) ;
#9669 = CARTESIAN_POINT ( 'NONE',  ( 194.0478494775925924, 31.85563505625661662, -14.00000000000006395 ) ) ;
#9670 = ORIENTED_EDGE ( 'NONE', *, *, #10637, .F. ) ;
#9671 =( NAMED_UNIT ( * ) PLANE_ANGLE_UNIT ( ) SI_UNIT ( $, .RADIAN. ) );
#9672 = AXIS2_PLACEMENT_3D ( 'NONE', #4660, #14541, #2004 ) ;
#9673 = CARTESIAN_POINT ( 'NONE',  ( 215.9829844511909300, 15.46048323788008361, -18.25196083293883120 ) ) ;
#9674 = EDGE_CURVE ( 'NONE', #4463, #5382, #10395, .T. ) ;
#9675 = CARTESIAN_POINT ( 'NONE',  ( 220.3643805408902381, 35.16445410620250556, -10.10863206319042362 ) ) ;
#9676 = DIRECTION ( 'NONE',  ( -0.5000000000000043299, 0.8660254037844360431, 0.000000000000000000 ) ) ;
#9677 = DIRECTION ( 'NONE',  ( 1.000000000000000000, 0.000000000000000000, -0.000000000000000000 ) ) ;
#9678 = ORIENTED_EDGE ( 'NONE', *, *, #17292, .T. ) ;
#9679 = VECTOR ( 'NONE', #13495, 1000.000000000000000 ) ;
#9680 = DIRECTION ( 'NONE',  ( 0.8944271909999204073, 0.000000000000000000, 0.4472135954999487684 ) ) ;
#9681 = PLANE ( 'NONE',  #4748 ) ;
#9682 = AXIS2_PLACEMENT_3D ( 'NONE', #4412, #12585, #20731 ) ;
#9683 = ORIENTED_EDGE ( 'NONE', *, *, #5654, .T. ) ;
#9684 = AXIS2_PLACEMENT_3D ( 'NONE', #8216, #3460, #2088 ) ;
#9685 = CARTESIAN_POINT ( 'NONE',  ( 99.99529059433426426, 150.7594456239217777, 21.00000000000000711 ) ) ;
#9686 = VERTEX_POINT ( 'NONE', #13620 ) ;
#9687 = CARTESIAN_POINT ( 'NONE',  ( 209.2403632168042975, 30.98959712955237578, -12.11805501175738620 ) ) ;
#9688 = CARTESIAN_POINT ( 'NONE',  ( 220.4346049221219346, 34.63089174143976834, -17.59730712095015193 ) ) ;
#9689 = CYLINDRICAL_SURFACE ( 'NONE', #241, 4.000000000000000000 ) ;
#9690 = DIRECTION ( 'NONE',  ( 0.03124427847888152504, -0.6611148994991491445, 0.7496338337632341142 ) ) ;
#9691 = CARTESIAN_POINT ( 'NONE',  ( -28.06779644517114036, 9.091084443369014778, -3.324986922928176547 ) ) ;
#9692 = ORIENTED_EDGE ( 'NONE', *, *, #3584, .T. ) ;
#9693 = VECTOR ( 'NONE', #18231, 1000.000000000000114 ) ;
#9694 = CIRCLE ( 'NONE', #12091, 12.47473710546057823 ) ;
#9695 = DIRECTION ( 'NONE',  ( 0.8426815769442687065, 0.4865224352899185645, 0.2306158707424266763 ) ) ;
#9696 = CARTESIAN_POINT ( 'NONE',  ( 209.3617675235332740, 26.90744277190043476, -9.718744748713266546 ) ) ;
#9697 = CARTESIAN_POINT ( 'NONE',  ( -5.193025761855540878, 45.33914674468751116, -6.290980308501477936 ) ) ;
#9698 = CARTESIAN_POINT ( 'NONE',  ( 203.5446072452137685, 23.54890371929340631, -14.00000000000005507 ) ) ;
#9699 = LINE ( 'NONE', #18091, #3378 ) ;
#9700 = CARTESIAN_POINT ( 'NONE',  ( 72.61279602124714927, 138.1873174624877265, 41.00000000000001421 ) ) ;
#9701 = EDGE_CURVE ( 'NONE', #1656, #4705, #9842, .T. ) ;
#9703 = ORIENTED_EDGE ( 'NONE', *, *, #7190, .T. ) ;
#9702 = EDGE_LOOP ( 'NONE', ( #1670, #17803, #13283, #11406, #8788 ) ) ;
#9704 = ORIENTED_EDGE ( 'NONE', *, *, #9727, .T. ) ;
#9705 = CARTESIAN_POINT ( 'NONE',  ( 191.0833833835253301, 36.99024094849632860, -9.087049258353282255 ) ) ;
#9706 = CARTESIAN_POINT ( 'NONE',  ( 227.5312376355471145, 39.64027283883993391, -14.00000000000005507 ) ) ;
#9707 = CARTESIAN_POINT ( 'NONE',  ( -7.003725213616844414, 79.78781110430779222, -9.858226064142291634 ) ) ;
#9708 = VERTEX_POINT ( 'NONE', #19852 ) ;
#9709 = ORIENTED_EDGE ( 'NONE', *, *, #18615, .T. ) ;
#9710 = ORIENTED_EDGE ( 'NONE', *, *, #14818, .F. ) ;
#9711 = VECTOR ( 'NONE', #4652, 1000.000000000000227 ) ;
#9712 = CARTESIAN_POINT ( 'NONE',  ( 219.1976456267619255, 35.05394349866926262, -17.56803216753788988 ) ) ;
#9713 = DIRECTION ( 'NONE',  ( -1.000000000000000000, -0.000000000000000000, -0.000000000000000000 ) ) ;
#9714 = CARTESIAN_POINT ( 'NONE',  ( -32.50512987981172586, 58.97167237099849757, 1.240746080457016509 ) ) ;
#9715 = DIRECTION ( 'NONE',  ( 0.000000000000000000, 0.000000000000000000, -1.000000000000000000 ) ) ;
#9716 = ORIENTED_EDGE ( 'NONE', *, *, #11585, .T. ) ;
#9717 = AXIS2_PLACEMENT_3D ( 'NONE', #16812, #2614, #9055 ) ;
#9718 = VERTEX_POINT ( 'NONE', #18590 ) ;
#9719 = DIRECTION ( 'NONE',  ( -0.5000000000000049960, 0.8660254037844358210, -0.000000000000000000 ) ) ;
#9720 = EDGE_CURVE ( 'NONE', #14936, #15611, #16983, .T. ) ;
#9721 = CARTESIAN_POINT ( 'NONE',  ( 5.000000000000000000, -4.685197434473809430, 6.071532165918824830E-15 ) ) ;
#9722 = CIRCLE ( 'NONE', #3993, 3.902363844300875240 ) ;
#9723 = CARTESIAN_POINT ( 'NONE',  ( 205.8264633344831225, 9.596613037118636669, -14.00000000000005507 ) ) ;
#9724 = CARTESIAN_POINT ( 'NONE',  ( -27.94575092597936816, 55.59861081455196086, 3.685053742613256578 ) ) ;
#9725 = CARTESIAN_POINT ( 'NONE',  ( 81.06711713768373784, 65.00000000000000000, -25.50000000000000000 ) ) ;
#9726 =( REPRESENTATION_RELATIONSHIP ('NONE','NONE', #4634, #10571 ) REPRESENTATION_RELATIONSHIP_WITH_TRANSFORMATION ( #3385 )SHAPE_REPRESENTATION_RELATIONSHIP( ) );
#9727 = EDGE_CURVE ( 'NONE', #12774, #14413, #7829, .T. ) ;
#9728 = ORIENTED_EDGE ( 'NONE', *, *, #4622, .F. ) ;
#9729 = AXIS2_PLACEMENT_3D ( 'NONE', #782, #15327, #13716 ) ;
#9730 = PLANE ( 'NONE',  #11159 ) ;
#9731 = CARTESIAN_POINT ( 'NONE',  ( 227.9553588074475670, 39.88513931160575510, -14.00000000000005507 ) ) ;
#9732 = ADVANCED_FACE ( 'NONE', ( #10408 ), #3740, .F. ) ;
#9733 = ORIENTED_EDGE ( 'NONE', *, *, #1664, .F. ) ;
#9734 = ORIENTED_EDGE ( 'NONE', *, *, #12767, .T. ) ;
#9735 = CARTESIAN_POINT ( 'NONE',  ( 62.29739936921044574, 78.35542098874827843, -12.12431711150143521 ) ) ;
#9736 = ORIENTED_EDGE ( 'NONE', *, *, #17593, .F. ) ;
#9737 = CARTESIAN_POINT ( 'NONE',  ( 207.9729903995531402, 4.459159050239305699, -1.722272971484193782 ) ) ;
#9738 = DIRECTION ( 'NONE',  ( 0.8660254037844360431, 0.5000000000000044409, -5.976026924694053325E-17 ) ) ;
#9739 = ORIENTED_EDGE ( 'NONE', *, *, #5564, .T. ) ;
#9740 = CARTESIAN_POINT ( 'NONE',  ( 205.0662616026534693, 10.91332106064940888, -14.00000000000005507 ) ) ;
#9741 = CONTEXT_DEPENDENT_SHAPE_REPRESENTATION ( #7283, #5847 ) ;
#9742 = CARTESIAN_POINT ( 'NONE',  ( 26.00000000000000355, 5.109226446042757607E-16, -4.171999999999999709 ) ) ;
#9743 = ORIENTED_EDGE ( 'NONE', *, *, #3189, .T. ) ;
#9744 = CARTESIAN_POINT ( 'NONE',  ( 218.6243502692013294, 37.76634477493627173, -16.35636678495280449 ) ) ;
#9745 = CARTESIAN_POINT ( 'NONE',  ( 208.9194833127196489, 31.78152281641241572, -14.00000000000007816 ) ) ;
#9746 = DIRECTION ( 'NONE',  ( -0.5000000000000025535, 0.8660254037844372643, 0.000000000000000000 ) ) ;
#9747 = CARTESIAN_POINT ( 'NONE',  ( 222.0023333938010524, 32.32743654455861559, -15.57898118447804769 ) ) ;
#9748 = CARTESIAN_POINT ( 'NONE',  ( 221.0163228795175030, 33.82927878612474615, -17.35168776101948751 ) ) ;
#9749 = EDGE_CURVE ( 'NONE', #20359, #15690, #10516, .T. ) ;
#9750 = CARTESIAN_POINT ( 'NONE',  ( 194.3181527907504176, 7.607334025971792535, -6.724618537539360119 ) ) ;
#9751 = CARTESIAN_POINT ( 'NONE',  ( 227.9553588074475670, 39.88513931160575510, -14.00000000000005507 ) ) ;
#9752 = CARTESIAN_POINT ( 'NONE',  ( 206.8805578665094345, 3.570835818144959539, -2.061577111287765440 ) ) ;
#9753 = AXIS2_PLACEMENT_3D ( 'NONE', #16057, #11158, #6266 ) ;
#9754 = EDGE_CURVE ( 'NONE', #15521, #18333, #2485, .T. ) ;
#9755 = VERTEX_POINT ( 'NONE', #20273 ) ;
#9756 = VERTEX_POINT ( 'NONE', #10088 ) ;
#9757 = DIRECTION ( 'NONE',  ( -1.000000000000000000, -0.000000000000000000, -0.000000000000000000 ) ) ;
#9758 = CARTESIAN_POINT ( 'NONE',  ( 65.44812640818317107, 80.19785434853127981, -3.638783230584851758 ) ) ;
#9759 = SHAPE_REPRESENTATION ( 'Drill Bit Indexing Pin', ( #18233 ), #3328 ) ;
#9760 = DIRECTION ( 'NONE',  ( -0.8660254037844370423, -0.5000000000000026645, 0.000000000000000000 ) ) ;
#9761 = CARTESIAN_POINT ( 'NONE',  ( 77.92638923178418509, 52.01750209009090042, -11.67654819968911717 ) ) ;
#9763 = ORIENTED_EDGE ( 'NONE', *, *, #10274, .T. ) ;
#9762 = ORIENTED_EDGE ( 'NONE', *, *, #19246, .F. ) ;
#9764 = ADVANCED_FACE ( 'NONE', ( #5737 ), #16691, .T. ) ;
#9765 = UNCERTAINTY_MEASURE_WITH_UNIT (LENGTH_MEASURE( 1.000000000000000082E-05 ), #4906, 'distance_accuracy_value', 'NONE');
#9766 = DIRECTION ( 'NONE',  ( 0.000000000000000000, 0.000000000000000000, -1.000000000000000000 ) ) ;
#9767 = CIRCLE ( 'NONE', #7411, 4.057500000000029416 ) ;
#9768 = ORIENTED_EDGE ( 'NONE', *, *, #14613, .T. ) ;
#9769 = CARTESIAN_POINT ( 'NONE',  ( 215.8017975273770332, 15.88692418043490306, -12.80378922971585887 ) ) ;
#9770 = CARTESIAN_POINT ( 'NONE',  ( -32.70858515791243093, 78.02673419565032020, -5.061054382488067382 ) ) ;
#9771 = CARTESIAN_POINT ( 'NONE',  ( 32.39721438298032297, 261.8427481158985870, -5.999999999999973355 ) ) ;
#9772 = EDGE_CURVE ( 'NONE', #3281, #11977, #18693, .T. ) ;
#9773 = ORIENTED_EDGE ( 'NONE', *, *, #15373, .T. ) ;
#9774 = CARTESIAN_POINT ( 'NONE',  ( -15.99999999999999289, 9.999999999999994671, 12.50000000000000000 ) ) ;
#9775 = EDGE_CURVE ( 'NONE', #6868, #12264, #19956, .T. ) ;
#9776 = CARTESIAN_POINT ( 'NONE',  ( 62.45290926645331098, 74.49313803559309122, -3.604012042188190268 ) ) ;
#9777 = DIRECTION ( 'NONE',  ( 0.5000000000000044409, -0.8660254037844360431, -4.006172263299080068E-16 ) ) ;
#9778 = VERTEX_POINT ( 'NONE', #17423 ) ;
#9779 = DIRECTION ( 'NONE',  ( 1.000000000000000000, 0.000000000000000000, 0.000000000000000000 ) ) ;
#9780 = PLANE ( 'NONE',  #20316 ) ;
#9781 = AXIS2_PLACEMENT_3D ( 'NONE', #18742, #4107, #20114 ) ;
#9782 = ORIENTED_EDGE ( 'NONE', *, *, #7741, .F. ) ;
#9783 = CARTESIAN_POINT ( 'NONE',  ( 22.00490953756709800, 255.8427481158984733, 1.000000000000028644 ) ) ;
#9784 = EDGE_CURVE ( 'NONE', #13943, #8036, #12660, .T. ) ;
#9785 = ORIENTED_EDGE ( 'NONE', *, *, #9794, .T. ) ;
#9786 = EDGE_CURVE ( 'NONE', #11719, #6269, #4858, .T. ) ;
#9787 = CARTESIAN_POINT ( 'NONE',  ( 210.6586702885180671, 28.45400361262161226, -11.82952947414952583 ) ) ;
#9788 = CARTESIAN_POINT ( 'NONE',  ( 218.3589628821741826, 38.22600921295526888, -15.50530648567712433 ) ) ;
#9789 = CARTESIAN_POINT ( 'NONE',  ( 216.7435376666127240, 9.522836875816564017, -21.90921222372436006 ) ) ;
#9790 = CIRCLE ( 'NONE', #6071, 3.902363844300875240 ) ;
#9791 = DIRECTION ( 'NONE',  ( 0.000000000000000000, -1.000000000000000000, 1.232415585510385534E-15 ) ) ;
#9792 = CARTESIAN_POINT ( 'NONE',  ( 10.49211908931699178, -10.00000000000000000, 0.000000000000000000 ) ) ;
#9793 = PLANE ( 'NONE',  #12692 ) ;
#9794 = EDGE_CURVE ( 'NONE', #15101, #15382, #9134, .T. ) ;
#9795 = ORIENTED_EDGE ( 'NONE', *, *, #3860, .F. ) ;
#9796 = CARTESIAN_POINT ( 'NONE',  ( 66.81417725909253136, 79.13633915520293272, -22.06525532588372585 ) ) ;
#9797 = AXIS2_PLACEMENT_3D ( 'NONE', #2922, #9364, #1541 ) ;
#9798 = CARTESIAN_POINT ( 'NONE',  ( -4.411380774409790817, 58.90144870373934083, 4.688306218574344264 ) ) ;
#9799 = VECTOR ( 'NONE', #598, 1000.000000000000000 ) ;
#9800 = ORIENTED_EDGE ( 'NONE', *, *, #16117, .F. ) ;
#9801 = CARTESIAN_POINT ( 'NONE',  ( 0.000000000000000000, 0.000000000000000000, 0.000000000000000000 ) ) ;
#9802 = CARTESIAN_POINT ( 'NONE',  ( -4.702552499873432268, 63.82970699952134197, 5.349554939795952535 ) ) ;
#9803 = CARTESIAN_POINT ( 'NONE',  ( -15.06548238822073671, 80.00001702854306984, -12.48688330620196929 ) ) ;
#9804 = ADVANCED_FACE ( 'NONE', ( #15640 ), #16321, .T. ) ;
#9805 = LINE ( 'NONE', #6620, #332 ) ;
#9806 = CYLINDRICAL_SURFACE ( 'NONE', #5277, 5.000000000000036415 ) ;
#9807 = VERTEX_POINT ( 'NONE', #15743 ) ;
#9808 = DIRECTION ( 'NONE',  ( -0.5000000000000027756, 0.8660254037844370423, -4.885182764539217401E-15 ) ) ;
#9809 = FACE_OUTER_BOUND ( 'NONE', #4625, .T. ) ;
#9810 = ORIENTED_EDGE ( 'NONE', *, *, #10362, .T. ) ;
#9811 = DIRECTION ( 'NONE',  ( -1.000000000000000000, 0.000000000000000000, 0.000000000000000000 ) ) ;
#9812 = B_SPLINE_CURVE_WITH_KNOTS ( 'NONE', 3,
 ( #11785, #11367, #16151, #6780 ),
 .UNSPECIFIED., .F., .F.,
 ( 4, 4 ),
 ( 3.206650225965500782E-07, 0.0004523739068024644982 ),
 .UNSPECIFIED. ) ;
#9813 = DIRECTION ( 'NONE',  ( 1.000000000000000000, 0.000000000000000000, 0.000000000000000000 ) ) ;
#9814 = CARTESIAN_POINT ( 'NONE',  ( 49.99529059433375267, 237.3619860023654553, 26.00000000000001776 ) ) ;
#9815 = AXIS2_PLACEMENT_3D ( 'NONE', #2266, #17208, #20169 ) ;
#9816 = CARTESIAN_POINT ( 'NONE',  ( 213.5401130648333492, 14.58114004716331280, -6.286464976499002155 ) ) ;
#9817 = ORIENTED_EDGE ( 'NONE', *, *, #1968, .T. ) ;
#9818 = VECTOR ( 'NONE', #8403, 1000.000000000000000 ) ;
#9819 = VERTEX_POINT ( 'NONE', #13936 ) ;
#9820 = CARTESIAN_POINT ( 'NONE',  ( 0.000000000000000000, 0.000000000000000000, 6.099999999999999645 ) ) ;
#9821 = VECTOR ( 'NONE', #10254, 1000.000000000000000 ) ;
#9822 = CARTESIAN_POINT ( 'NONE',  ( 220.6021407664647995, 34.10476814008172397, -17.30537846547898795 ) ) ;
#9823 = VECTOR ( 'NONE', #18719, 1000.000000000000114 ) ;
#9824 = CONICAL_SURFACE ( 'NONE', #377, 13.07248899748297433, 0.6693469023067423196 ) ;
#9825 = CARTESIAN_POINT ( 'NONE',  ( 197.9399629305378880, -1.336196318472940181, -14.00519586093461832 ) ) ;
#9826 = DIRECTION ( 'NONE',  ( -0.5000000000000034417, 0.8660254037844364872, 0.000000000000000000 ) ) ;
#9827 = CYLINDRICAL_SURFACE ( 'NONE', #442, 5.000000000000036415 ) ;
#9828 = AXIS2_PLACEMENT_3D ( 'NONE', #8010, #5043, #19460 ) ;
#9829 = CARTESIAN_POINT ( 'NONE',  ( 66.19073749086841474, 149.3106491262846589, 41.00000000000001421 ) ) ;
#9830 = VECTOR ( 'NONE', #6169, 1000.000000000000000 ) ;
#9831 = CARTESIAN_POINT ( 'NONE',  ( 28.00000000000001066, 65.75000000000001421, 1.479896280015810639 ) ) ;
#9832 = EDGE_LOOP ( 'NONE', ( #2337, #14218, #20301, #16552 ) ) ;
#9833 = CARTESIAN_POINT ( 'NONE',  ( 63.34582467611540579, 77.73072509497566784, -8.044670883999552657 ) ) ;
#9834 = VERTEX_POINT ( 'NONE', #12552 ) ;
#9835 = CARTESIAN_POINT ( 'NONE',  ( 215.5644888513662067, 15.74991395245902304, -11.24974199967302013 ) ) ;
#9836 = CARTESIAN_POINT ( 'NONE',  ( 199.5722073119862046, -0.9062415656482646353, -8.625373497621064089 ) ) ;
#9837 = ORIENTED_EDGE ( 'NONE', *, *, #5090, .T. ) ;
#9838 = LINE ( 'NONE', #3597, #6987 ) ;
#9839 = ORIENTED_EDGE ( 'NONE', *, *, #7877, .F. ) ;
#9840 = AXIS2_PLACEMENT_3D ( 'NONE', #2690, #7651, #14037 ) ;
#9841 = CONICAL_SURFACE ( 'NONE', #728, 10.85470691220533190, 0.8171114040043576665 ) ;
#9842 = CIRCLE ( 'NONE', #3427, 5.000000000000005329 ) ;
#9843 = CARTESIAN_POINT ( 'NONE',  ( 213.9139752855751055, 14.44296291959195955, -21.91826003371448905 ) ) ;
#9844 = EDGE_LOOP ( 'NONE', ( #10511, #13176, #14857, #12777 ) ) ;
#9845 = ADVANCED_FACE ( 'NONE', ( #1204 ), #15538, .F. ) ;
#9846 = DIRECTION ( 'NONE',  ( 0.000000000000000000, 0.000000000000000000, -1.000000000000000000 ) ) ;
#9847 = CARTESIAN_POINT ( 'NONE',  ( 208.8107687779841228, 4.427644383670616079, -14.00000000000005507 ) ) ;
#9848 = CYLINDRICAL_SURFACE ( 'NONE', #5933, 5.000000000000001776 ) ;
#9849 = CARTESIAN_POINT ( 'NONE',  ( 205.0662616026534693, 10.91332106064940888, -14.00000000000005507 ) ) ;
#9850 = ORIENTED_EDGE ( 'NONE', *, *, #7346, .F. ) ;
#9851 = CARTESIAN_POINT ( 'NONE',  ( -28.99999999999999289, 0.000000000000000000, -15.00000000000000000 ) ) ;
#9852 = LINE ( 'NONE', #9439, #7898 ) ;
#9853 = PLANE ( 'NONE',  #12251 ) ;
#9854 = ORIENTED_EDGE ( 'NONE', *, *, #9615, .T. ) ;
#9855 = CIRCLE ( 'NONE', #14973, 0.9999999999999917843 ) ;
#9856 = DIRECTION ( 'NONE',  ( -0.5000000000000054401, 0.8660254037844354880, -0.000000000000000000 ) ) ;
#9857 = CARTESIAN_POINT ( 'NONE',  ( 67.66310225583265492, 78.47357137787466286, -2.555409790234332235 ) ) ;
#9858 = EDGE_CURVE ( 'NONE', #1521, #20014, #1107, .T. ) ;
#9859 = VECTOR ( 'NONE', #7550, 1000.000000000000000 ) ;
#9860 = CARTESIAN_POINT ( 'NONE',  ( 206.8720745992954164, 3.565938001535339907, -25.93669565428267276 ) ) ;
#9861 = CARTESIAN_POINT ( 'NONE',  ( 75.90040729020685717, 53.15606728486817190, -7.041156951942071807 ) ) ;
#9863 = ORIENTED_EDGE ( 'NONE', *, *, #15060, .T. ) ;
#9862 = ORIENTED_EDGE ( 'NONE', *, *, #20095, .F. ) ;
#9864 = VERTEX_POINT ( 'NONE', #2594 ) ;
#9865 = ORIENTED_EDGE ( 'NONE', *, *, #4106, .T. ) ;
#9866 = EDGE_CURVE ( 'NONE', #5485, #734, #10730, .T. ) ;
#9867 = FACE_OUTER_BOUND ( 'NONE', #2890, .T. ) ;
#9868 = VERTEX_POINT ( 'NONE', #995 ) ;
#9869 = B_SPLINE_CURVE_WITH_KNOTS ( 'NONE', 3,
 ( #1249, #7696, #14197, #4529 ),
 .UNSPECIFIED., .F., .F.,
 ( 4, 4 ),
 ( 9.410049375302480474E-05, 0.0007667512858034030571 ),
 .UNSPECIFIED. ) ;
#9870 = CARTESIAN_POINT ( 'NONE',  ( 196.9311089575304266, 4.991927054840251010, -20.59651891138145174 ) ) ;
#9871 = EDGE_CURVE ( 'NONE', #3527, #13130, #7438, .T. ) ;
#9872 = AXIS2_PLACEMENT_3D ( 'NONE', #6910, #12016, #18377 ) ;
#9873 = FACE_OUTER_BOUND ( 'NONE', #5360, .T. ) ;
#9874 = DIRECTION ( 'NONE',  ( 0.5000000000000049960, -0.8660254037844358210, 0.000000000000000000 ) ) ;
#9875 = AXIS2_PLACEMENT_3D ( 'NONE', #7263, #18410, #8432 ) ;
#9876 = ADVANCED_FACE ( 'NONE', ( #14263 ), #14043, .T. ) ;
#9877 = CARTESIAN_POINT ( 'NONE',  ( 54.74529948059490891, 77.78781281343189846, -14.84991977410729191 ) ) ;
#9878 = CARTESIAN_POINT ( 'NONE',  ( 221.3540177668497222, 33.45035214977922777, -10.82724490084735791 ) ) ;
#9879 = EDGE_LOOP ( 'NONE', ( #5447, #7949, #2400, #19573 ) ) ;
#9880 = FACE_OUTER_BOUND ( 'NONE', #9250, .T. ) ;
#9881 = DIRECTION ( 'NONE',  ( -0.000000000000000000, -1.000000000000000000, -0.000000000000000000 ) ) ;
#9882 = VERTEX_POINT ( 'NONE', #4383 ) ;
#9883 = DIRECTION ( 'NONE',  ( 0.8660254037844369313, 0.5000000000000029976, 4.996003610813203446E-16 ) ) ;
#9884 = VECTOR ( 'NONE', #12962, 1000.000000000000114 ) ;
#9885 = ADVANCED_FACE ( 'NONE', ( #6059 ), #5953, .T. ) ;
#9886 = AXIS2_PLACEMENT_3D ( 'NONE', #16898, #15230, #18494 ) ;
#9887 = EDGE_LOOP ( 'NONE', ( #13393, #10878, #7261 ) ) ;
#9888 = CARTESIAN_POINT ( 'NONE',  ( 210.3223930243060238, 28.95850756564502859, -11.57946969169901763 ) ) ;
#9889 = CARTESIAN_POINT ( 'NONE',  ( 227.9553588074475670, 39.88513931160575510, -14.00000000000005507 ) ) ;
#9890 = CARTESIAN_POINT ( 'NONE',  ( 209.6243204174557206, 3.018531609524862880, -14.00000000000005507 ) ) ;
#9891 = EDGE_CURVE ( 'NONE', #3202, #10176, #1312, .T. ) ;
#9892 = DIRECTION ( 'NONE',  ( 0.000000000000000000, 0.000000000000000000, 1.000000000000000000 ) ) ;
#9893 = CARTESIAN_POINT ( 'NONE',  ( 49.99529059433375267, 237.3619860023654553, 26.00000000000001776 ) ) ;
#9894 = LINE ( 'NONE', #3446, #4881 ) ;
#9895 = ORIENTED_EDGE ( 'NONE', *, *, #19505, .F. ) ;
#9896 = CARTESIAN_POINT ( 'NONE',  ( 61.57468973143931379, 74.87077495648827608, -20.95977551465545119 ) ) ;
#9897 = CARTESIAN_POINT ( 'NONE',  ( 97.00490953756778367, 125.9389375482329569, -29.00000000000002487 ) ) ;
#9898 = CONICAL_SURFACE ( 'NONE', #3490, 10.85470691220533190, 0.8171114040043576665 ) ;
#9899 = EDGE_CURVE ( 'NONE', #8008, #1440, #553, .T. ) ;
#9900 = ADVANCED_FACE ( 'NONE', ( #2802 ), #13477, .F. ) ;
#9901 = EDGE_LOOP ( 'NONE', ( #3437, #6085, #17325, #15213 ) ) ;
#9902 = DIRECTION ( 'NONE',  ( 0.5000000000000049960, -0.8660254037844358210, 0.000000000000000000 ) ) ;
#9903 = CARTESIAN_POINT ( 'NONE',  ( -3.497189663385620761, 49.35567744637351240, -0.02171244038980547214 ) ) ;
#9904 = CARTESIAN_POINT ( 'NONE',  ( 77.00490953756764156, 160.5799536996104280, 26.00000000000001066 ) ) ;
#9905 = DIRECTION ( 'NONE',  ( -1.000000000000000000, 0.000000000000000000, 0.000000000000000000 ) ) ;
#9906 = CARTESIAN_POINT ( 'NONE',  ( 5.000000000000004441, 2.342598717236899830, -4.057500000000030305 ) ) ;
#9908 = ORIENTED_EDGE ( 'NONE', *, *, #11564, .T. ) ;
#9907 = VERTEX_POINT ( 'NONE', #13689 ) ;
#9909 = ORIENTED_EDGE ( 'NONE', *, *, #9617, .F. ) ;
#9910 = DIRECTION ( 'NONE',  ( -0.000000000000000000, -0.000000000000000000, 1.000000000000000000 ) ) ;
#9911 = DIRECTION ( 'NONE',  ( -0.5000000000000008882, 0.8660254037844381525, 0.000000000000000000 ) ) ;
#9912 = EDGE_CURVE ( 'NONE', #9495, #11054, #16753, .T. ) ;
#9913 = ORIENTED_EDGE ( 'NONE', *, *, #17144, .F. ) ;
#9914 = CARTESIAN_POINT ( 'NONE',  ( -17.87065464597074893, 58.81735738840291106, -4.639596491434944348 ) ) ;
#9915 = CARTESIAN_POINT ( 'NONE',  ( 198.5622009498131604, -1.489369010732141785, -13.97827067520021593 ) ) ;
#9916 = CARTESIAN_POINT ( 'NONE',  ( 218.4367820612134494, 37.88530424025100984, -12.10162843130809840 ) ) ;
#9917 = CARTESIAN_POINT ( 'NONE',  ( -16.00000000000007105, 58.38562172233837089, -4.999999999999997335 ) ) ;
#9918 = AXIS2_PLACEMENT_3D ( 'NONE', #15880, #14199, #6100 ) ;
#9919 = ORIENTED_EDGE ( 'NONE', *, *, #6546, .T. ) ;
#9920 = ORIENTED_EDGE ( 'NONE', *, *, #12513, .T. ) ;
#9921 = CARTESIAN_POINT ( 'NONE',  ( 157.3972143829815309, 45.33639716978955647, -6.000000000000052403 ) ) ;
#9922 = ADVANCED_FACE ( 'NONE', ( #10477 ), #12315, .T. ) ;
#9923 = EDGE_LOOP ( 'NONE', ( #16825, #16991, #8926, #30 ) ) ;
#9924 = ORIENTED_EDGE ( 'NONE', *, *, #376, .T. ) ;
#9925 = DIRECTION ( 'NONE',  ( -0.8660254037844360431, -0.5000000000000045519, -4.336808689942050277E-16 ) ) ;
#9926 = EDGE_CURVE ( 'NONE', #20835, #19075, #5795, .T. ) ;
#9927 = DIRECTION ( 'NONE',  ( -0.8601696498176549799, -0.4966191788709765631, 0.1160929141252379365 ) ) ;
#9928 = CARTESIAN_POINT ( 'NONE',  ( -28.68049345341341194, 53.83925212050883857, -2.471093196081551646 ) ) ;
#9929 = LINE ( 'NONE', #18115, #12305 ) ;
#9930 = AXIS2_PLACEMENT_3D ( 'NONE', #12956, #1603, #11350 ) ;
#9931 = AXIS2_PLACEMENT_3D ( 'NONE', #12204, #5924, #18776 ) ;
#9932 = ORIENTED_EDGE ( 'NONE', *, *, #19352, .F. ) ;
#9933 = DIRECTION ( 'NONE',  ( 1.000000000000000000, 0.000000000000000000, 0.000000000000000000 ) ) ;
#9934 = LINE ( 'NONE', #11543, #9332 ) ;
#9935 = ORIENTED_EDGE ( 'NONE', *, *, #19252, .F. ) ;
#9936 = CARTESIAN_POINT ( 'NONE',  ( 64.60297720430702384, 80.85304810415020427, -4.137593906014268796 ) ) ;
#9937 = VERTEX_POINT ( 'NONE', #959 ) ;
#9938 = CARTESIAN_POINT ( 'NONE',  ( -4.702542490863385716, 65.65291453363785479, 5.349528374469380232 ) ) ;
#9939 = LINE ( 'NONE', #6445, #20503 ) ;
#9940 = EDGE_LOOP ( 'NONE', ( #13228, #12978, #8460, #10527, #4829, #19783 ) ) ;
#9941 = CARTESIAN_POINT ( 'NONE',  ( 228.8647755551524483, 38.30998329932686630, -17.45257705044836172 ) ) ;
#9942 = CARTESIAN_POINT ( 'NONE',  ( -28.94448814640270129, 65.74999999999995737, 3.385962996190683860 ) ) ;
#9943 = ORIENTED_EDGE ( 'NONE', *, *, #2940, .F. ) ;
#9944 = CARTESIAN_POINT ( 'NONE',  ( 64.99529059433392320, 211.3812238888322952, 11.00000000000001066 ) ) ;
#9945 = DIRECTION ( 'NONE',  ( -0.8660254037844355990, -0.5000000000000055511, 0.000000000000000000 ) ) ;
#9946 = CARTESIAN_POINT ( 'NONE',  ( 221.7369802378075860, 32.16919332334362025, -13.95097276009443910 ) ) ;
#9947 = FACE_OUTER_BOUND ( 'NONE', #6822, .T. ) ;
#9948 = EDGE_LOOP ( 'NONE', ( #19226, #6292, #11319, #9782 ) ) ;
#9949 = CARTESIAN_POINT ( 'NONE',  ( 199.2144802262915846, 21.04890371929339921, -14.00000000000005507 ) ) ;
#9950 = DIRECTION ( 'NONE',  ( 0.8660254037844374864, 0.5000000000000021094, 2.220446049250313081E-16 ) ) ;
#9951 = CARTESIAN_POINT ( 'NONE',  ( 221.9501777499663717, 32.21179470361161634, -12.94403591235904116 ) ) ;
#9952 = ORIENTED_EDGE ( 'NONE', *, *, #19632, .T. ) ;
#9953 = DIRECTION ( 'NONE',  ( 0.7499999999999953371, 0.4330127018922228510, -0.5000000000000038858 ) ) ;
#9954 = CARTESIAN_POINT ( 'NONE',  ( 203.0967589511048743, 24.15675494531242506, -13.08406428195295668 ) ) ;
#9955 = EDGE_CURVE ( 'NONE', #12709, #1466, #15299, .T. ) ;
#9956 = CARTESIAN_POINT ( 'NONE',  ( -15.81957430612866311, 71.61437827766145858, -4.999999999999988454 ) ) ;
#9957 = CARTESIAN_POINT ( 'NONE',  ( 75.38983945845171775, 52.47636342738726256, -9.003451077243985523 ) ) ;
#9959 = VERTEX_POINT ( 'NONE', #13790 ) ;
#9958 = VERTEX_POINT ( 'NONE', #17078 ) ;
#9960 = VERTEX_POINT ( 'NONE', #20140 ) ;
#9961 = VERTEX_POINT ( 'NONE', #7097 ) ;
#9962 = DIRECTION ( 'NONE',  ( 0.5000000000000044409, -0.8660254037844360431, -4.006172263299080068E-16 ) ) ;
#9963 = VERTEX_POINT ( 'NONE', #5601 ) ;
#9964 = CARTESIAN_POINT ( 'NONE',  ( 199.2144802262915846, 21.04890371929339921, -14.00000000000005507 ) ) ;
#9965 = CLOSED_SHELL ( 'NONE', ( #2365, #3631, #13510, #880, #6018, #4465, #1491, #10128, #7948, #12257, #5267, #3449, #19496, #2436, #14879, #20049, #16348, #3826, #10519, #8852, #5369, #4982, #4805, #7016, #8871, #20543, #3813, #9363, #9272, #18112, #7562, #18886, #2314, #12193, #5894, #9876, #4214, #17579, #754, #13660, #12085, #11019, #15237, #10889, #16490, #3536, #15631, #19643, #5762, #4252, #8525, #1506, #4382, #2886, #13659, #4709, #7057, #6288, #4354, #4490, #8988, #19204, #12410, #15727, #13325, #109, #16381, #19832, #17069, #11106, #12929, #10945, #7526, #17068, #6901, #18868, #3666, #10279, #18820, #14135, #19856, #13817, #19509, #5340, #10691, #605, #887, #1790, #4610, #985, #1636, #15988, #16168, #9845, #20703, #19031, #5455, #10919, #6758, #17920, #18681, #10618, #5224, #16432, #14982, #4978, #7853, #17301, #6146, #11720, #19258, #9065, #1867, #12366, #16756, #16047, #13054, #8474, #17530, #5963, #5479, #882, #11887, #1348, #19136, #10036, #7957, #19448, #18424, #234, #19473, #11225, #7719, #6773, #4123, #15010, #1959, #6744, #13508, #19527, #2354, #20423, #13150, #9319, #12842, #6342, #8601, #15229, #11852, #12798, #5917, #11293, #4108, #20267, #6405, #4989, #9804, #16051, #16058, #19342, #19109, #1825, #5120, #360, #15326, #12409, #11283, #12857, #13574, #19393, #5856, #12296, #16880, #13041, #3391, #16640, #15644, #2308, #17171, #11711, #11603, #10981, #10292, #14035, #17290, #2549, #593 ) ) ;
#9966 = CARTESIAN_POINT ( 'NONE',  ( -21.63278055428463276, 79.98685641808557989, -11.85964839587038000 ) ) ;
#9967 = CARTESIAN_POINT ( 'NONE',  ( 220.9606893667113638, 33.51376855353427686, -16.94731950718130520 ) ) ;
#9968 = PLANE ( 'NONE',  #19970 ) ;
#9969 = ORIENTED_EDGE ( 'NONE', *, *, #11860, .T. ) ;
#9970 = EDGE_CURVE ( 'NONE', #12271, #14150, #2236, .T. ) ;
#9971 = CIRCLE ( 'NONE', #8646, 9.999999999999998224 ) ;
#9972 = CARTESIAN_POINT ( 'NONE',  ( 213.7874248973967610, 18.84792351767029572, -16.70797078425240656 ) ) ;
#9973 = CARTESIAN_POINT ( 'NONE',  ( 79.20327082793765783, 66.58182770179300292, 0.4060056306182541763 ) ) ;
#9974 = DIRECTION ( 'NONE',  ( -0.8660254037844360431, -0.5000000000000044409, 5.976026924694052093E-17 ) ) ;
#9975 = ORIENTED_EDGE ( 'NONE', *, *, #1363, .F. ) ;
#9976 = PLANE ( 'NONE',  #6768 ) ;
#9977 = EDGE_CURVE ( 'NONE', #20099, #11291, #7402, .T. ) ;
#9978 = CARTESIAN_POINT ( 'NONE',  ( 218.1772659767879361, 38.33479928385730062, -13.56204498775452372 ) ) ;
#9979 = EDGE_CURVE ( 'NONE', #2271, #8514, #8861, .T. ) ;
#9980 = CIRCLE ( 'NONE', #19470, 13.99999999999999822 ) ;
#9981 = DIRECTION ( 'NONE',  ( -1.000000000000000000, 0.000000000000000000, 0.000000000000000000 ) ) ;
#9982 = ORIENTED_EDGE ( 'NONE', *, *, #13837, .F. ) ;
#9983 = CONICAL_SURFACE ( 'NONE', #3928, 10.85470691220533190, 0.8171114040043576665 ) ;
#9984 = LINE ( 'NONE', #6921, #7827 ) ;
#9985 = CARTESIAN_POINT ( 'NONE',  ( 4.000000000000000000, 3.518949890710767026, -4.987329993433320396E-15 ) ) ;
#9986 = VECTOR ( 'NONE', #5919, 1000.000000000000227 ) ;
#9987 = DIRECTION ( 'NONE',  ( 0.4953429730181667656, -0.8579591964396799941, 0.1361666490962538667 ) ) ;
#9988 = CARTESIAN_POINT ( 'NONE',  ( 82.53324728627625007, 64.66165602865051198, -25.62270589083005845 ) ) ;
#9989 = DIRECTION ( 'NONE',  ( 0.1503837331804444566, 0.08682408883347132733, 0.9848077530122061329 ) ) ;
#9990 = ORIENTED_EDGE ( 'NONE', *, *, #2788, .T. ) ;
#9991 = CARTESIAN_POINT ( 'NONE',  ( 80.95562266652501648, 67.15461460196840449, -25.59299666572612963 ) ) ;
#9992 = VECTOR ( 'NONE', #14813, 1000.000000000000000 ) ;
#9993 = DIRECTION ( 'NONE',  ( 0.4999999999999995004, -0.8660254037844390407, 0.000000000000000000 ) ) ;
#9994 = ADVANCED_FACE ( 'NONE', ( #3919 ), #18449, .F. ) ;
#9995 = VERTEX_POINT ( 'NONE', #13894 ) ;
#9996 = VECTOR ( 'NONE', #10121, 999.9999999999998863 ) ;
#9997 = CYLINDRICAL_SURFACE ( 'NONE', #3479, 7.155882939242646401 ) ;
#9998 = CARTESIAN_POINT ( 'NONE',  ( 1.503934470862336559, 53.26675808472690932, -3.147798062369893124 ) ) ;
#9999 = CARTESIAN_POINT ( 'NONE',  ( -15.99999999999999289, 9.999999999999994671, -17.50000000000000000 ) ) ;
#10000 = VECTOR ( 'NONE', #1590, 1000.000000000000000 ) ;
#10001 = DIRECTION ( 'NONE',  ( 0.8660254037844352659, 0.5000000000000056621, 0.000000000000000000 ) ) ;
#10002 = EDGE_CURVE ( 'NONE', #8080, #3911, #13613, .T. ) ;
#10003 = CARTESIAN_POINT ( 'NONE',  ( 229.0363929556513369, 37.03326735113697055, -16.48323849494068227 ) ) ;
#10004 = CARTESIAN_POINT ( 'NONE',  ( 205.8564897284660731, 2.721990579170014080, -25.44774858730788125 ) ) ;
#10006 = ORIENTED_EDGE ( 'NONE', *, *, #20871, .T. ) ;
#10005 = ORIENTED_EDGE ( 'NONE', *, *, #17402, .F. ) ;
#10007 = ORIENTED_EDGE ( 'NONE', *, *, #20131, .F. ) ;
#10008 = ORIENTED_EDGE ( 'NONE', *, *, #4339, .T. ) ;
#10009 = CARTESIAN_POINT ( 'NONE',  ( 226.6211368133091923, 39.11482588413117867, -14.00000000000005507 ) ) ;
#10010 = DIRECTION ( 'NONE',  ( 0.8660254037844360431, 0.5000000000000044409, -5.976026924694053325E-17 ) ) ;
#10011 = EDGE_CURVE ( 'NONE', #8085, #12773, #20240, .T. ) ;
#10012 = ORIENTED_EDGE ( 'NONE', *, *, #17646, .T. ) ;
#10013 = EDGE_LOOP ( 'NONE', ( #20207, #19435, #635, #1863 ) ) ;
#10014 = VERTEX_POINT ( 'NONE', #16968 ) ;
#10015 = CARTESIAN_POINT ( 'NONE',  ( -16.88984037207102062, 58.47342245001757277, -4.923257761629218798 ) ) ;
#10016 = CARTESIAN_POINT ( 'NONE',  ( 197.3517780161357678, 19.97347209683980296, -26.28791492288515386 ) ) ;
#10017 = CARTESIAN_POINT ( 'NONE',  ( -15.81983077554147421, 58.38562172233856273, -4.999999999999992895 ) ) ;
#10018 = ORIENTED_EDGE ( 'NONE', *, *, #15607, .F. ) ;
#10019 = EDGE_CURVE ( 'NONE', #5664, #7029, #10265, .T. ) ;
#10020 = ORIENTED_EDGE ( 'NONE', *, *, #10333, .T. ) ;
#10021 = CONICAL_SURFACE ( 'NONE', #12438, 4.509097725792825528, 0.5235987755983015912 ) ;
#10022 = CARTESIAN_POINT ( 'NONE',  ( 227.5312376355471145, 39.64027283883993391, -14.00000000000005507 ) ) ;
#10023 = ORIENTED_EDGE ( 'NONE', *, *, #13292, .T. ) ;
#10024 = FACE_OUTER_BOUND ( 'NONE', #4895, .T. ) ;
#10025 = EDGE_CURVE ( 'NONE', #16603, #18065, #16992, .T. ) ;
#10026 = FACE_OUTER_BOUND ( 'NONE', #17629, .T. ) ;
#10027 = CARTESIAN_POINT ( 'NONE',  ( -28.90575499228997103, 55.17197461462945540, -1.140010367715231343 ) ) ;
#10028 = CARTESIAN_POINT ( 'NONE',  ( -18.65171524015568139, 19.34141692181273342, 12.21627542118126541 ) ) ;
#10029 = EDGE_CURVE ( 'NONE', #3306, #4564, #12934, .T. ) ;
#10030 = CARTESIAN_POINT ( 'NONE',  ( 5.000000000000004441, 4.685197434473814759, -6.938893903907228378E-15 ) ) ;
#10031 = LINE ( 'NONE', #13141, #8321 ) ;
#10032 = AXIS2_PLACEMENT_3D ( 'NONE', #5383, #16957, #11985 ) ;
#10033 = VECTOR ( 'NONE', #3074, 1000.000000000000114 ) ;
#10034 = ORIENTED_EDGE ( 'NONE', *, *, #9277, .F. ) ;
#10035 = ORIENTED_EDGE ( 'NONE', *, *, #7124, .F. ) ;
#10036 = ADVANCED_FACE ( 'NONE', ( #15190 ), #15086, .F. ) ;
#10037 = CARTESIAN_POINT ( 'NONE',  ( 58.19665357825395802, 76.31805631966230408, -6.092558036382285991 ) ) ;
#10038 = ORIENTED_EDGE ( 'NONE', *, *, #11869, .F. ) ;
#10039 = VERTEX_POINT ( 'NONE', #13586 ) ;
#10040 = ORIENTED_EDGE ( 'NONE', *, *, #14071, .F. ) ;
#10041 = FACE_OUTER_BOUND ( 'NONE', #11583, .T. ) ;
#10042 = DIRECTION ( 'NONE',  ( 0.1674398060854926096, -0.2900142513495593821, -0.9422609221188190665 ) ) ;
#10043 = EDGE_CURVE ( 'NONE', #12385, #18641, #2342, .T. ) ;
#10044 = EDGE_LOOP ( 'NONE', ( #10839, #11979, #18223, #1381, #14482 ) ) ;
#10045 = CARTESIAN_POINT ( 'NONE',  ( 190.7433706042750146, 35.72129598111152404, -19.00000000000003908 ) ) ;
#10046 = EDGE_CURVE ( 'NONE', #6001, #1760, #14225, .T. ) ;
#10047 = CARTESIAN_POINT ( 'NONE',  ( -30.87525101170383124, 65.74999999999997158, 2.549678278787586461 ) ) ;
#10048 = ORIENTED_EDGE ( 'NONE', *, *, #4236, .T. ) ;
#10049 = AXIS2_PLACEMENT_3D ( 'NONE', #14080, #12694, #2935 ) ;
#10050 = B_SPLINE_CURVE_WITH_KNOTS ( 'NONE', 3,
 ( #5596, #20033, #8794, #5913 ),
 .UNSPECIFIED., .F., .F.,
 ( 4, 4 ),
 ( 3.169130416727337534E-07, 0.0005858052687812691662 ),
 .UNSPECIFIED. ) ;
#10051 = PRODUCT_DEFINITION_SHAPE ( 'NONE', 'NONE',  #5599 ) ;
#10052 = DIRECTION ( 'NONE',  ( 0.5000000000000045519, -0.8660254037844362651, 0.000000000000000000 ) ) ;
#10053 = DIRECTION ( 'NONE',  ( -0.5000000000000054401, 0.8660254037844354880, -0.000000000000000000 ) ) ;
#10054 = EDGE_CURVE ( 'NONE', #18580, #1937, #7635, .T. ) ;
#10055 = VECTOR ( 'NONE', #19432, 1000.000000000000114 ) ;
#10056 = FACE_OUTER_BOUND ( 'NONE', #1362, .T. ) ;
#10057 = PLANE ( 'NONE',  #17361 ) ;
#10058 = VERTEX_POINT ( 'NONE', #4557 ) ;
#10059 = DIRECTION ( 'NONE',  ( 0.4999999999999995004, -0.8660254037844390407, 0.000000000000000000 ) ) ;
#10060 = CARTESIAN_POINT ( 'NONE',  ( 206.1736271717860234, 10.32809743383080558, -25.81526893633800412 ) ) ;
#10061 = CARTESIAN_POINT ( 'NONE',  ( 218.0611881365336444, 9.768376490446161853, -19.34736286182901210 ) ) ;
#10062 = ORIENTED_EDGE ( 'NONE', *, *, #150, .T. ) ;
#10063 = EDGE_CURVE ( 'NONE', #20133, #11936, #6231, .T. ) ;
#10064 = DIRECTION ( 'NONE',  ( 0.8660254037844371533, 0.5000000000000025535, -6.106226635438359986E-16 ) ) ;
#10065 = DIRECTION ( 'NONE',  ( 0.000000000000000000, 0.6933752452815372669, 0.7205766921228913269 ) ) ;
#10066 = LINE ( 'NONE', #14884, #20305 ) ;
#10067 = CARTESIAN_POINT ( 'NONE',  ( 80.60295752769052058, 52.96396996839209237, -20.75661811798801892 ) ) ;
#10068 = VECTOR ( 'NONE', #18585, 1000.000000000000114 ) ;
#10070 = VERTEX_POINT ( 'NONE', #11023 ) ;
#10069 = VERTEX_POINT ( 'NONE', #7624 ) ;
#10071 = B_SPLINE_CURVE_WITH_KNOTS ( 'NONE', 3,
 ( #14496, #9688, #16273, #14707 ),
 .UNSPECIFIED., .F., .F.,
 ( 4, 4 ),
 ( 2.764878223288369275E-07, 0.0004523297296022177382 ),
 .UNSPECIFIED. ) ;
#10072 = ORIENTED_EDGE ( 'NONE', *, *, #10460, .T. ) ;
#10073 = PLANE ( 'NONE',  #4950 ) ;
#10074 = ORIENTED_EDGE ( 'NONE', *, *, #13024, .F. ) ;
#10075 = CARTESIAN_POINT ( 'NONE',  ( 80.90185716406490712, 60.51308707325554792, -24.71776202822431046 ) ) ;
#10076 = CARTESIAN_POINT ( 'NONE',  ( -24.99627478638403844, 79.78781110430777801, -9.858226064141845768 ) ) ;
#10077 = CARTESIAN_POINT ( 'NONE',  ( 227.1116836665104302, 41.34642752079204087, -17.14987233279964585 ) ) ;
#10078 = CARTESIAN_POINT ( 'NONE',  ( 201.7914626300884890, 0.3750460896586316206, -22.62267072728657524 ) ) ;
#10079 = ORIENTED_EDGE ( 'NONE', *, *, #1240, .T. ) ;
#10080 = AXIS2_PLACEMENT_3D ( 'NONE', #15484, #12706, #18753 ) ;
#10081 = DIRECTION ( 'NONE',  ( 1.000000000000000000, 0.000000000000000000, 0.000000000000000000 ) ) ;
#10082 = AXIS2_PLACEMENT_3D ( 'NONE', #19938, #12007, #18573 ) ;
#10083 = CARTESIAN_POINT ( 'NONE',  ( 54.42754686098177075, 77.92279056475767618, -13.93489572546247857 ) ) ;
#10084 = CARTESIAN_POINT ( 'NONE',  ( -15.99999999999999289, 80.00000000000000000, -4.999999999999989342 ) ) ;
#10085 = ORIENTED_EDGE ( 'NONE', *, *, #5344, .F. ) ;
#10086 = CARTESIAN_POINT ( 'NONE',  ( 228.4171206443014910, 38.10587845811534180, -10.52303454827241502 ) ) ;
#10087 = FACE_OUTER_BOUND ( 'NONE', #12180, .T. ) ;
#10088 = CARTESIAN_POINT ( 'NONE',  ( 207.3262688097345574, 1.076026043308923930, -14.00000000000005507 ) ) ;
#10089 = CARTESIAN_POINT ( 'NONE',  ( -7.939600225062636518, 79.94564677075823056, -11.17290160265476473 ) ) ;
#10090 = ORIENTED_EDGE ( 'NONE', *, *, #18211, .F. ) ;
#10091 = VECTOR ( 'NONE', #13607, 1000.000000000000000 ) ;
#10092 = EDGE_CURVE ( 'NONE', #3560, #6339, #2089, .T. ) ;
#10093 = CARTESIAN_POINT ( 'NONE',  ( 193.5622009498131035, 7.170885027112213983, -13.97827067520021416 ) ) ;
#10094 = DIRECTION ( 'NONE',  ( -0.4999999999999995004, 0.8660254037844390407, 0.000000000000000000 ) ) ;
#10095 = LINE ( 'NONE', #7033, #7322 ) ;
#10096 = CARTESIAN_POINT ( 'NONE',  ( 81.55002576568772099, 66.38583373074199301, -25.62495068049236835 ) ) ;
#10097 = CARTESIAN_POINT ( 'NONE',  ( -29.99999999999979039, 5.000000000000201617, 0.4679281238166860257 ) ) ;
#10098 =( NAMED_UNIT ( * ) PLANE_ANGLE_UNIT ( ) SI_UNIT ( $, .RADIAN. ) );
#10099 = CARTESIAN_POINT ( 'NONE',  ( -31.74999999999995737, 0.000000000000000000, 0.000000000000000000 ) ) ;
#10100 = ORIENTED_EDGE ( 'NONE', *, *, #19742, .F. ) ;
#10101 = EDGE_CURVE ( 'NONE', #13861, #3576, #2764, .T. ) ;
#10102 = CARTESIAN_POINT ( 'NONE',  ( 78.66618490269718222, 56.96778211784575774, -22.73333863286613266 ) ) ;
#10103 = CARTESIAN_POINT ( 'NONE',  ( -7.000292895910345869, 44.98883621322416104, -8.709882378375517931 ) ) ;
#10104 = AXIS2_PLACEMENT_3D ( 'NONE', #12511, #18557, #5817 ) ;
#10105 = ORIENTED_EDGE ( 'NONE', *, *, #8614, .F. ) ;
#10106 = FACE_OUTER_BOUND ( 'NONE', #7945, .T. ) ;
#10107 = CARTESIAN_POINT ( 'NONE',  ( -3.048040018689400110, 56.82851019708963491, 0.1106114228930126370 ) ) ;
#10108 = FACE_OUTER_BOUND ( 'NONE', #12349, .T. ) ;
#10109 = DIRECTION ( 'NONE',  ( 0.8660254037844359321, 0.5000000000000046629, 0.000000000000000000 ) ) ;
#10110 = CARTESIAN_POINT ( 'NONE',  ( -15.99999999999999289, 80.00000000000000000, -12.50000000000000000 ) ) ;
#10111 = CARTESIAN_POINT ( 'NONE',  ( 205.3647371392095806, 3.210897180031505371, -25.94618751764486575 ) ) ;
#10113 = ORIENTED_EDGE ( 'NONE', *, *, #4437, .F. ) ;
#10112 = VERTEX_POINT ( 'NONE', #3069 ) ;
#10114 = ORIENTED_EDGE ( 'NONE', *, *, #624, .T. ) ;
#10115 = DIRECTION ( 'NONE',  ( -0.4926956718456823592, 0.8533739363059945626, -0.1703053134172390071 ) ) ;
#10116 = FACE_OUTER_BOUND ( 'NONE', #2351, .T. ) ;
#10117 = EDGE_CURVE ( 'NONE', #1421, #10783, #2096, .T. ) ;
#10118 = VERTEX_POINT ( 'NONE', #6132 ) ;
#10119 = CARTESIAN_POINT ( 'NONE',  ( 195.2863413965735333, 4.042320060767385037, -12.62152863576138806 ) ) ;
#10120 = FACE_OUTER_BOUND ( 'NONE', #7922, .T. ) ;
#10121 = DIRECTION ( 'NONE',  ( 0.4758887346169385357, 0.2747544890354034486, -0.8354878114129393740 ) ) ;
#10122 = VERTEX_POINT ( 'NONE', #5918 ) ;
#10123 = CARTESIAN_POINT ( 'NONE',  ( 78.05328906524978549, 52.67459052937854835, 0.6180898526239277935 ) ) ;
#10124 = CARTESIAN_POINT ( 'NONE',  ( 182.3972143829816446, 2.035126980567696364, -22.00000000000003908 ) ) ;
#10125 = VECTOR ( 'NONE', #16914, 1000.000000000000000 ) ;
#10126 = EDGE_CURVE ( 'NONE', #11067, #7581, #13466, .T. ) ;
#10127 = CONICAL_SURFACE ( 'NONE', #15266, 13.07248899748297433, 0.6693469023067423196 ) ;
#10128 = ADVANCED_FACE ( 'NONE', ( #9100 ), #12720, .T. ) ;
#10129 = FACE_OUTER_BOUND ( 'NONE', #13772, .T. ) ;
#10130 = CARTESIAN_POINT ( 'NONE',  ( 209.6971420603676677, 12.36239970324706050, -2.990331769139234375 ) ) ;
#10131 = CARTESIAN_POINT ( 'NONE',  ( -28.48657445126280763, 48.50183867280838257, -0.8242875664313024098 ) ) ;
#10132 = DIRECTION ( 'NONE',  ( 0.8660254037844380415, 0.5000000000000014433, 0.000000000000000000 ) ) ;
#10133 = B_SPLINE_CURVE_WITH_KNOTS ( 'NONE', 3,
 ( #11748, #18209, #638, #20314 ),
 .UNSPECIFIED., .F., .F.,
 ( 4, 4 ),
 ( 3.532015366367899196E-07, 0.0004524064433164875013 ),
 .UNSPECIFIED. ) ;
#10134 = FACE_OUTER_BOUND ( 'NONE', #11173, .T. ) ;
#10135 = DIRECTION ( 'NONE',  ( 0.000000000000000000, 1.224646799147353207E-16, 1.000000000000000000 ) ) ;
#10136 = EDGE_CURVE ( 'NONE', #12995, #20836, #19183, .T. ) ;
#10138 = EDGE_LOOP ( 'NONE', ( #19239, #2028, #11217, #11110 ) ) ;
#10137 = ORIENTED_EDGE ( 'NONE', *, *, #307, .T. ) ;
#10139 = VECTOR ( 'NONE', #17525, 1000.000000000000227 ) ;
#10140 = CARTESIAN_POINT ( 'NONE',  ( 62.90137823179582455, 78.00269638309853804, -12.54667390848797837 ) ) ;
#10141 = AXIS2_PLACEMENT_3D ( 'NONE', #6916, #8829, #5536 ) ;
#10142 = EDGE_LOOP ( 'NONE', ( #15612, #4054, #4509 ) ) ;
#10143 = DIRECTION ( 'NONE',  ( -0.4999999999999995004, 0.8660254037844390407, 0.000000000000000000 ) ) ;
#10144 = CARTESIAN_POINT ( 'NONE',  ( 8.000000000000000000, 0.000000000000000000, 0.000000000000000000 ) ) ;
#10145 = ADVANCED_FACE ( 'NONE', ( #7727 ), #4655, .T. ) ;
#10146 = CONICAL_SURFACE ( 'NONE', #697, 10.85470691220533190, 0.8171114040043576665 ) ;
#10147 = ORIENTED_EDGE ( 'NONE', *, *, #19759, .T. ) ;
#10148 = DIRECTION ( 'NONE',  ( 1.000000000000000000, 0.000000000000000000, 0.000000000000000000 ) ) ;
#10149 = EDGE_CURVE ( 'NONE', #1834, #12562, #7359, .T. ) ;
#10150 = CYLINDRICAL_SURFACE ( 'NONE', #818, 1.499999999999993783 ) ;
#10151 = VERTEX_POINT ( 'NONE', #7927 ) ;
#10152 = AXIS2_PLACEMENT_3D ( 'NONE', #3403, #9856, #8059 ) ;
#10153 = DIRECTION ( 'NONE',  ( 1.000000000000000000, 0.000000000000000000, 0.000000000000000000 ) ) ;
#10154 = CARTESIAN_POINT ( 'NONE',  ( 227.3709454187517451, 40.89737299345080146, -17.42570676230487337 ) ) ;
#10155 = AXIS2_PLACEMENT_3D ( 'NONE', #17898, #9808, #283 ) ;
#10156 = CARTESIAN_POINT ( 'NONE',  ( 228.1721461148598280, 38.53018678966859056, -17.68583624946730737 ) ) ;
#10157 = LINE ( 'NONE', #6887, #7638 ) ;
#10158 = CARTESIAN_POINT ( 'NONE',  ( 207.6891655446386551, 10.67204465957205350, -26.28791492288521781 ) ) ;
#10159 = VECTOR ( 'NONE', #5047, 1000.000000000000227 ) ;
#10160 = EDGE_CURVE ( 'NONE', #7321, #8661, #14009, .T. ) ;
#10161 = DIRECTION ( 'NONE',  ( -0.5000000000000041078, 0.8660254037844363761, 0.000000000000000000 ) ) ;
#10162 = DIRECTION ( 'NONE',  ( -0.8660254037844357100, -0.5000000000000051070, 0.000000000000000000 ) ) ;
#10163 = DIRECTION ( 'NONE',  ( 0.3886714912512298503, 0.2243995901002338311, 0.8936326403234118310 ) ) ;
#10164 = EDGE_CURVE ( 'NONE', #734, #9504, #17176, .T. ) ;
#10165 = EDGE_LOOP ( 'NONE', ( #10733, #12891, #20727, #18913, #2818 ) ) ;
#10166 = CARTESIAN_POINT ( 'NONE',  ( -1.115519630330159551, 65.75000000000000000, 2.547625675852271510 ) ) ;
#10167 = CIRCLE ( 'NONE', #6446, 11.98469917212512215 ) ;
#10168 = CIRCLE ( 'NONE', #5094, 12.47473710546057823 ) ;
#10169 = CARTESIAN_POINT ( 'NONE',  ( -12.70096667698038928, 69.85981968218749216, -3.758841495318840042 ) ) ;
#10170 = AXIS2_PLACEMENT_3D ( 'NONE', #16050, #1198, #18794 ) ;
#10171 = CARTESIAN_POINT ( 'NONE',  ( 78.40297945836096005, 52.91941870341079834, -7.572629818528286094 ) ) ;
#10172 = EDGE_CURVE ( 'NONE', #15099, #14795, #6829, .T. ) ;
#10174 = ORIENTED_EDGE ( 'NONE', *, *, #3972, .F. ) ;
#10173 = ORIENTED_EDGE ( 'NONE', *, *, #12429, .T. ) ;
#10175 = VECTOR ( 'NONE', #7682, 1000.000000000000227 ) ;
#10176 = VERTEX_POINT ( 'NONE', #12515 ) ;
#10177 = B_SPLINE_CURVE_WITH_KNOTS ( 'NONE', 3,
 ( #15367, #5355, #19999, #15157 ),
 .UNSPECIFIED., .F., .F.,
 ( 4, 4 ),
 ( 7.909111589570312167E-06, 0.0005738353338881527731 ),
 .UNSPECIFIED. ) ;
#10178 = AXIS2_PLACEMENT_3D ( 'NONE', #6734, #16108, #4948 ) ;
#10179 = DIRECTION ( 'NONE',  ( 0.2597919750177185572, -0.4499729001293500397, -0.8544194045464879039 ) ) ;
#10180 = ORIENTED_EDGE ( 'NONE', *, *, #118, .T. ) ;
#10181 = CARTESIAN_POINT ( 'NONE',  ( 75.48021121295072078, 52.59641686382532555, -16.40691147115069626 ) ) ;
#10182 = EDGE_CURVE ( 'NONE', #17941, #14915, #18976, .T. ) ;
#10183 = DIRECTION ( 'NONE',  ( -1.000000000000000000, -0.000000000000000000, -0.000000000000000000 ) ) ;
#10184 = CARTESIAN_POINT ( 'NONE',  ( 202.1791022559531541, 13.45620526910692227, -29.00000000000009237 ) ) ;
#10185 = CARTESIAN_POINT ( 'NONE',  ( 218.4997737894814804, 38.18806966980842788, -15.94147978600224391 ) ) ;
#10186 = VERTEX_POINT ( 'NONE', #15809 ) ;
#10187 = VECTOR ( 'NONE', #19858, 1000.000000000000227 ) ;
#10188 = CARTESIAN_POINT ( 'NONE',  ( 220.8589169312680838, 34.30789195187642093, -17.68583624946730737 ) ) ;
#10189 = AXIS2_PLACEMENT_3D ( 'NONE', #11010, #17479, #4645 ) ;
#10190 = VECTOR ( 'NONE', #4862, 1000.000000000000114 ) ;
#10191 = DIRECTION ( 'NONE',  ( -0.5000000000000054401, 0.8660254037844354880, -0.000000000000000000 ) ) ;
#10192 = LINE ( 'NONE', #8400, #17882 ) ;
#10193 = VERTEX_POINT ( 'NONE', #16322 ) ;
#10194 = DIRECTION ( 'NONE',  ( 1.000000000000000000, 0.000000000000000000, 0.000000000000000000 ) ) ;
#10195 = CARTESIAN_POINT ( 'NONE',  ( 94.31531706421118599, 208.0571376747316492, 11.00000000000001066 ) ) ;
#10196 = DIRECTION ( 'NONE',  ( 0.5000000000000044409, -0.8660254037844360431, -4.006172263299080068E-16 ) ) ;
#10197 = CARTESIAN_POINT ( 'NONE',  ( -2.899236859673289146, 78.36047030499231880, -5.510874449651578466 ) ) ;
#10198 = VECTOR ( 'NONE', #2380, 1000.000000000000227 ) ;
#10200 = EDGE_LOOP ( 'NONE', ( #6577, #20229, #19613, #14332 ) ) ;
#10199 = ORIENTED_EDGE ( 'NONE', *, *, #18715, .T. ) ;
#10201 = ORIENTED_EDGE ( 'NONE', *, *, #218, .T. ) ;
#10202 = PLANE ( 'NONE',  #16320 ) ;
#10203 = CARTESIAN_POINT ( 'NONE',  ( 219.8932653677503026, 35.56851935375815543, -10.32863559915724672 ) ) ;
#10204 = DIRECTION ( 'NONE',  ( 0.8296432542242785368, 0.4789947561577507784, 0.2868032327110803803 ) ) ;
#10205 = VECTOR ( 'NONE', #17336, 1000.000000000000227 ) ;
#10206 = AXIS2_PLACEMENT_3D ( 'NONE', #13242, #14646, #2000 ) ;
#10207 = DIRECTION ( 'NONE',  ( 0.5000000000000055511, -0.8660254037844353769, 2.220446049250313574E-16 ) ) ;
#10208 = CARTESIAN_POINT ( 'NONE',  ( -26.75565744063416318, 9.893465008606606048, 6.378074558502260238 ) ) ;
#10209 =( NAMED_UNIT ( * ) PLANE_ANGLE_UNIT ( ) SI_UNIT ( $, .RADIAN. ) );
#10210 = DIRECTION ( 'NONE',  ( -1.000000000000000000, -0.000000000000000000, -0.000000000000000000 ) ) ;
#10211 = ORIENTED_EDGE ( 'NONE', *, *, #4082, .T. ) ;
#10212 = CARTESIAN_POINT ( 'NONE',  ( 80.02304891312839175, 59.01526275525436915, -24.05071924315015153 ) ) ;
#10213 = CARTESIAN_POINT ( 'NONE',  ( -3.927421424228952684, 54.52359887367414615, 3.254349035475716967 ) ) ;
#10214 = ORIENTED_EDGE ( 'NONE', *, *, #3697, .T. ) ;
#10215 = DIRECTION ( 'NONE',  ( 0.5000000000000051070, -0.8660254037844359321, 0.000000000000000000 ) ) ;
#10216 = CARTESIAN_POINT ( 'NONE',  ( -4.579482833895355931, 60.98411661173300047, 5.082820002145302496 ) ) ;
#10217 = CARTESIAN_POINT ( 'NONE',  ( -3.572474243005702821, 79.61902841131316677, -9.096985201275369803 ) ) ;
#10218 = AXIS2_PLACEMENT_3D ( 'NONE', #4482, #4372, #20579 ) ;
#10219 = DIRECTION ( 'NONE',  ( 0.5000000000000054401, -0.8660254037844354880, -1.665334536937734318E-16 ) ) ;
#10220 = CARTESIAN_POINT ( 'NONE',  ( 210.3654177961080052, 6.098041503423209164, -1.717498466822859227 ) ) ;
#10221 = DIRECTION ( 'NONE',  ( -0.8660254037844355990, -0.5000000000000055511, 0.000000000000000000 ) ) ;
#10223 = ORIENTED_EDGE ( 'NONE', *, *, #20711, .T. ) ;
#10222 = ORIENTED_EDGE ( 'NONE', *, *, #4508, .F. ) ;
#10224 = VERTEX_POINT ( 'NONE', #200 ) ;
#10225 = CARTESIAN_POINT ( 'NONE',  ( 221.7369802378075860, 32.16919332334362025, -13.95097276009443910 ) ) ;
#10226 = DIRECTION ( 'NONE',  ( -0.8660254037844362651, -0.5000000000000045519, 5.976026924694053325E-17 ) ) ;
#10227 = VERTEX_POINT ( 'NONE', #19387 ) ;
#10228 = EDGE_CURVE ( 'NONE', #19879, #5830, #16497, .T. ) ;
#10229 = CARTESIAN_POINT ( 'NONE',  ( 81.54035229546286700, 64.23212122210442487, 0.4788660375907791700 ) ) ;
#10230 = PRODUCT_DEFINITION_SHAPE ( 'NONE', 'NONE',  #20954 ) ;
#10231 = CARTESIAN_POINT ( 'NONE',  ( 86.00000000000000000, 65.00000000000000000, -2.500000000000005773 ) ) ;
#10232 = DIRECTION ( 'NONE',  ( -0.8660254037844355990, -0.5000000000000055511, 0.000000000000000000 ) ) ;
#10233 = ORIENTED_EDGE ( 'NONE', *, *, #10025, .T. ) ;
#10234 = PLANE ( 'NONE',  #18472 ) ;
#10235 = CARTESIAN_POINT ( 'NONE',  ( 208.5625094892126583, 11.70731928285941770, -25.48492467622476099 ) ) ;
#10236 = VECTOR ( 'NONE', #16120, 1000.000000000000114 ) ;
#10237 = VERTEX_POINT ( 'NONE', #12935 ) ;
#10238 = CARTESIAN_POINT ( 'NONE',  ( 85.37797649651368204, 230.0773763115391262, -28.99999999999998934 ) ) ;
#10239 = EDGE_CURVE ( 'NONE', #15949, #8848, #11333, .T. ) ;
#10240 = DIRECTION ( 'NONE',  ( 1.000000000000000000, 0.000000000000000000, -1.124692329640370702E-16 ) ) ;
#10241 = CARTESIAN_POINT ( 'NONE',  ( -31.15489049490080475, 50.26056083818948395, -9.697909921291566704 ) ) ;
#10242 = DIRECTION ( 'NONE',  ( -0.3886714912512189701, -0.2243995901002275584, 0.8936326403234180482 ) ) ;
#10243 = VERTEX_POINT ( 'NONE', #5058 ) ;
#10244 = DIRECTION ( 'NONE',  ( 0.5000000000000049960, -0.8660254037844358210, 0.000000000000000000 ) ) ;
#10245 = FACE_OUTER_BOUND ( 'NONE', #8573, .T. ) ;
#10247 = VERTEX_POINT ( 'NONE', #4754 ) ;
#10246 = ORIENTED_EDGE ( 'NONE', *, *, #20356, .T. ) ;
#10248 = AXIS2_PLACEMENT_3D ( 'NONE', #4683, #16049, #14775 ) ;
#10249 = CARTESIAN_POINT ( 'NONE',  ( 54.25673667531765432, 77.99532872960556062, -12.93714471232228647 ) ) ;
#10250 = EDGE_CURVE ( 'NONE', #19586, #527, #14951, .T. ) ;
#10251 = ORIENTED_EDGE ( 'NONE', *, *, #11700, .T. ) ;
#10252 = EDGE_CURVE ( 'NONE', #20929, #13537, #16118, .T. ) ;
#10253 = ORIENTED_EDGE ( 'NONE', *, *, #9586, .T. ) ;
#10254 = DIRECTION ( 'NONE',  ( -0.7071067811865331398, 0.000000000000000000, 0.7071067811865620056 ) ) ;
#10255 = DIRECTION ( 'NONE',  ( 0.000000000000000000, 0.000000000000000000, 1.000000000000000000 ) ) ;
#10256 = ORIENTED_EDGE ( 'NONE', *, *, #7335, .F. ) ;
#10257 = CARTESIAN_POINT ( 'NONE',  ( 86.00000000000000000, 65.00000000000000000, 0.4999999999999970024 ) ) ;
#10258 = ORIENTED_EDGE ( 'NONE', *, *, #5788, .F. ) ;
#10259 = CARTESIAN_POINT ( 'NONE',  ( 213.7342555843919740, 14.51621837890814248, -21.80597602412992231 ) ) ;
#10260 = ORIENTED_EDGE ( 'NONE', *, *, #14833, .T. ) ;
#10261 = VECTOR ( 'NONE', #9116, 1000.000000000000000 ) ;
#10262 = CARTESIAN_POINT ( 'NONE',  ( 227.9553588074475954, 39.88513931160571957, -14.00000000000005507 ) ) ;
#10263 = CONICAL_SURFACE ( 'NONE', #15054, 3.047499999999999876, 1.047197551196590748 ) ;
#10264 = LINE ( 'NONE', #3390, #9315 ) ;
#10265 = LINE ( 'NONE', #12197, #10887 ) ;
#10266 = CARTESIAN_POINT ( 'NONE',  ( 219.8596994420543922, 35.21110819772844991, -14.00000000000005507 ) ) ;
#10267 = DIRECTION ( 'NONE',  ( 1.000000000000000000, 0.000000000000000000, 0.000000000000000000 ) ) ;
#10268 = EDGE_CURVE ( 'NONE', #2368, #10684, #3777, .T. ) ;
#10269 = LINE ( 'NONE', #3820, #5006 ) ;
#10270 = CARTESIAN_POINT ( 'NONE',  ( 208.9513496856693564, 16.05581419235814522, -3.762296834228893605 ) ) ;
#10271 = CARTESIAN_POINT ( 'NONE',  ( 205.0662616026534693, 10.91332106064940888, -14.00000000000005507 ) ) ;
#10272 = ORIENTED_EDGE ( 'NONE', *, *, #4582, .F. ) ;
#10273 = CARTESIAN_POINT ( 'NONE',  ( 219.6109973649995197, 35.85150367506854963, -10.49174204642374519 ) ) ;
#10274 = EDGE_CURVE ( 'NONE', #6959, #15695, #3171, .T. ) ;
#10275 = VERTEX_POINT ( 'NONE', #13136 ) ;
#10276 = FACE_OUTER_BOUND ( 'NONE', #4778, .T. ) ;
#10277 = VECTOR ( 'NONE', #13733, 1000.000000000000000 ) ;
#10278 = DIRECTION ( 'NONE',  ( -0.8660254037844357100, -0.5000000000000053291, 0.000000000000000000 ) ) ;
#10279 = ADVANCED_FACE ( 'NONE', ( #8236 ), #1, .F. ) ;
#10281 = EDGE_LOOP ( 'NONE', ( #7311, #4692, #18086, #15251 ) ) ;
#10280 = ORIENTED_EDGE ( 'NONE', *, *, #12591, .F. ) ;
#10282 = EDGE_CURVE ( 'NONE', #8359, #6033, #5143, .T. ) ;
#10283 = DIRECTION ( 'NONE',  ( 0.000000000000000000, 0.000000000000000000, 1.000000000000000000 ) ) ;
#10284 = EDGE_CURVE ( 'NONE', #7653, #6420, #1686, .T. ) ;
#10285 = VERTEX_POINT ( 'NONE', #8133 ) ;
#10286 = CARTESIAN_POINT ( 'NONE',  ( 75.03375843245487431, 52.00451211173042054, -12.01334687468304985 ) ) ;
#10287 = CARTESIAN_POINT ( 'NONE',  ( -25.37873435132391009, 79.74334935823260651, -9.599827418924029132 ) ) ;
#10288 = CARTESIAN_POINT ( 'NONE',  ( 198.4659246047362444, -1.544954184478863901, -13.98474561060102772 ) ) ;
#10289 = DIRECTION ( 'NONE',  ( 0.000000000000000000, 0.000000000000000000, -1.000000000000000000 ) ) ;
#10290 = VERTEX_POINT ( 'NONE', #13037 ) ;
#10291 = DIRECTION ( 'NONE',  ( 0.000000000000000000, 0.000000000000000000, -1.000000000000000000 ) ) ;
#10292 = ADVANCED_FACE ( 'NONE', ( #10026 ), #19703, .T. ) ;
#10293 = CARTESIAN_POINT ( 'NONE',  ( 195.6198561393837281, 4.234874887307574554, -16.70797078425209037 ) ) ;
#10294 = LINE ( 'NONE', #15425, #6350 ) ;
#10295 = ORIENTED_EDGE ( 'NONE', *, *, #16540, .F. ) ;
#10296 = FACE_OUTER_BOUND ( 'NONE', #3690, .T. ) ;
#10297 = DIRECTION ( 'NONE',  ( -0.000000000000000000, 1.000000000000000000, -0.000000000000000000 ) ) ;
#10298 = DIRECTION ( 'NONE',  ( 0.8660254037844355990, 0.5000000000000054401, 3.017578575841809918E-14 ) ) ;
#10299 = LINE ( 'NONE', #7339, #16209 ) ;
#10300 = EDGE_CURVE ( 'NONE', #6800, #15885, #19476, .T. ) ;
#10302 = EDGE_LOOP ( 'NONE', ( #11587, #242, #14835, #15855 ) ) ;
#10301 = ORIENTED_EDGE ( 'NONE', *, *, #4581, .F. ) ;
#10303 = ORIENTED_EDGE ( 'NONE', *, *, #8772, .F. ) ;
#10304 = CYLINDRICAL_SURFACE ( 'NONE', #17332, 5.999999999999998224 ) ;
#10305 = LINE ( 'NONE', #15231, #14289 ) ;
#10306 = CARTESIAN_POINT ( 'NONE',  ( -0.1767699604045824824, 65.74999999999997158, 2.481238266578629226 ) ) ;
#10307 = EDGE_CURVE ( 'NONE', #310, #11827, #3581, .T. ) ;
#10308 = CARTESIAN_POINT ( 'NONE',  ( 79.40833726504349954, 49.63029741583935106, -14.45290996621378277 ) ) ;
#10309 = ADVANCED_FACE ( 'NONE', ( #19581 ), #8448, .T. ) ;
#10310 = VECTOR ( 'NONE', #1977, 1000.000000000000227 ) ;
#10311 = CARTESIAN_POINT ( 'NONE',  ( -29.99999999999999645, 5.000000000000000000, 10.50000000000000711 ) ) ;
#10312 = FACE_OUTER_BOUND ( 'NONE', #16099, .T. ) ;
#10313 = VERTEX_POINT ( 'NONE', #18012 ) ;
#10314 = EDGE_CURVE ( 'NONE', #8036, #17291, #3482, .T. ) ;
#10315 = B_SPLINE_CURVE_WITH_KNOTS ( 'NONE', 3,
 ( #12415, #11986, #14004, #16961 ),
 .UNSPECIFIED., .F., .F.,
 ( 4, 4 ),
 ( 2.736592200848096035E-07, 0.0005857620149597167133 ),
 .UNSPECIFIED. ) ;
#10316 = CARTESIAN_POINT ( 'NONE',  ( 82.34777263834683936, 58.50307748515720618, -24.38835257526326927 ) ) ;
#10317 = DIRECTION ( 'NONE',  ( 1.000000000000000000, 0.000000000000000000, 0.000000000000000000 ) ) ;
#10318 = EDGE_CURVE ( 'NONE', #11249, #3359, #300, .T. ) ;
#10319 = EDGE_LOOP ( 'NONE', ( #191, #16955, #17407, #9839 ) ) ;
#10320 = CARTESIAN_POINT ( 'NONE',  ( 202.1920911364529445, 25.46077609459828750, -15.45182294182971283 ) ) ;
#10321 = CARTESIAN_POINT ( 'NONE',  ( -0.1881451998551312010, 64.85124100632805266, 2.499262340588669584 ) ) ;
#10322 = CARTESIAN_POINT ( 'NONE',  ( 214.8600158830803650, 14.81213703278996618, -20.84195174293595443 ) ) ;
#10323 = B_SPLINE_CURVE_WITH_KNOTS ( 'NONE', 3,
 ( #12417, #20549, #9098, #6022 ),
 .UNSPECIFIED., .F., .F.,
 ( 4, 4 ),
 ( 8.676057312167167649E-07, 0.0005667938280123673359 ),
 .UNSPECIFIED. ) ;
#10324 = CARTESIAN_POINT ( 'NONE',  ( -34.00000000000000711, 64.25000000000000000, 2.481238266578627449 ) ) ;
#10325 = CARTESIAN_POINT ( 'NONE',  ( 205.8264633344831225, 9.596613037118636669, -14.00000000000005507 ) ) ;
#10326 = DIRECTION ( 'NONE',  ( 0.000000000000000000, -0.9359693004502194214, 0.3520816220917059036 ) ) ;
#10327 = CIRCLE ( 'NONE', #11697, 5.000000000000005329 ) ;
#10329 = ORIENTED_EDGE ( 'NONE', *, *, #4219, .T. ) ;
#10328 = ORIENTED_EDGE ( 'NONE', *, *, #10136, .T. ) ;
#10330 = EDGE_LOOP ( 'NONE', ( #16762, #87, #316 ) ) ;
#10331 = VECTOR ( 'NONE', #2024, 1000.000000000000227 ) ;
#10332 = FACE_OUTER_BOUND ( 'NONE', #17605, .T. ) ;
#10333 = EDGE_CURVE ( 'NONE', #11978, #1958, #416, .T. ) ;
#10334 = DIRECTION ( 'NONE',  ( 0.6958540455341891695, 0.000000000000000000, -0.7181832268395738073 ) ) ;
#10335 = VERTEX_POINT ( 'NONE', #15474 ) ;
#10336 = ORIENTED_EDGE ( 'NONE', *, *, #15536, .F. ) ;
#10337 = CARTESIAN_POINT ( 'NONE',  ( 227.9553588074475954, 39.88513931160571957, -14.00000000000005507 ) ) ;
#10338 = DIRECTION ( 'NONE',  ( -0.2883401610574364282, 0.4994198088140709424, 0.8169698930104392076 ) ) ;
#10339 = ORIENTED_EDGE ( 'NONE', *, *, #15388, .F. ) ;
#10340 = DIRECTION ( 'NONE',  ( 0.8660254037844358210, 0.5000000000000046629, 0.000000000000000000 ) ) ;
#10341 = CARTESIAN_POINT ( 'NONE',  ( 61.99529059433385925, 216.5773763115390125, -22.00000000000000355 ) ) ;
#10342 = AXIS2_PLACEMENT_3D ( 'NONE', #7587, #10764, #12481 ) ;
#10343 = VECTOR ( 'NONE', #6144, 1000.000000000000000 ) ;
#10344 = CIRCLE ( 'NONE', #9672, 2.499999999999997780 ) ;
#10345 = CARTESIAN_POINT ( 'NONE',  ( 157.3972143829815309, 45.33639716978955647, -6.000000000000052403 ) ) ;
#10346 = ADVANCED_FACE ( 'NONE', ( #20115 ), #3790, .T. ) ;
#10347 = FACE_OUTER_BOUND ( 'NONE', #19799, .T. ) ;
#10348 = CARTESIAN_POINT ( 'NONE',  ( -26.82492178207555611, 45.34741445055429665, -6.259914210700230797 ) ) ;
#10349 = DIRECTION ( 'NONE',  ( 0.3878556453522130631, -0.6717856837524455171, -0.6310879443260485333 ) ) ;
#10350 = ORIENTED_EDGE ( 'NONE', *, *, #20306, .F. ) ;
#10351 = CARTESIAN_POINT ( 'NONE',  ( 218.6234151596997322, 10.86579850426016769, -9.718744748713266546 ) ) ;
#10352 = LINE ( 'NONE', #523, #2926 ) ;
#10353 = ORIENTED_EDGE ( 'NONE', *, *, #6403, .F. ) ;
#10354 = AXIS2_PLACEMENT_3D ( 'NONE', #16563, #2045, #10283 ) ;
#10355 = CARTESIAN_POINT ( 'NONE',  ( 62.68497280389577497, 78.12921337523277998, -12.39230198697897833 ) ) ;
#10356 = ORIENTED_EDGE ( 'NONE', *, *, #2573, .F. ) ;
#10357 = ORIENTED_EDGE ( 'NONE', *, *, #16067, .T. ) ;
#10358 = AXIS2_PLACEMENT_3D ( 'NONE', #14529, #19278, #4746 ) ;
#10359 = ORIENTED_EDGE ( 'NONE', *, *, #10239, .F. ) ;
#10360 = CARTESIAN_POINT ( 'NONE',  ( 198.8591165883520659, 24.81846684157315508, -14.00000000000005507 ) ) ;
#10361 = CARTESIAN_POINT ( 'NONE',  ( 227.9553588074475670, 39.88513931160575510, -14.00000000000005507 ) ) ;
#10362 = EDGE_CURVE ( 'NONE', #17399, #2569, #6162, .T. ) ;
#10363 = ORIENTED_EDGE ( 'NONE', *, *, #16398, .F. ) ;
#10364 = VERTEX_POINT ( 'NONE', #10130 ) ;
#10365 = DIRECTION ( 'NONE',  ( 0.5000000000000031086, -0.8660254037844368202, 0.000000000000000000 ) ) ;
#10366 = LINE ( 'NONE', #15396, #19904 ) ;
#10367 = DIRECTION ( 'NONE',  ( 0.8660254037844374864, 0.5000000000000018874, 8.326672684688672821E-17 ) ) ;
#10368 = DIRECTION ( 'NONE',  ( 0.000000000000000000, 6.938893903907178303E-18, 1.000000000000000000 ) ) ;
#10369 = CONICAL_SURFACE ( 'NONE', #1262, 10.85470691220533190, 0.8171114040043576665 ) ;
#10370 = ADVANCED_FACE ( 'NONE', ( #5576 ), #15061, .T. ) ;
#10371 = CARTESIAN_POINT ( 'NONE',  ( 32.36389338619004263, 157.9004617752989930, -12.50000000000000000 ) ) ;
#10372 = DIRECTION ( 'NONE',  ( -0.5000000000000051070, 0.8660254037844359321, -0.000000000000000000 ) ) ;
#10373 = FACE_OUTER_BOUND ( 'NONE', #14777, .T. ) ;
#10374 = VERTEX_POINT ( 'NONE', #620 ) ;
#10375 = FACE_OUTER_BOUND ( 'NONE', #5902, .T. ) ;
#10376 = EDGE_CURVE ( 'NONE', #10497, #6334, #20726, .T. ) ;
#10377 = CARTESIAN_POINT ( 'NONE',  ( 4.000000000000000000, 0.000000000000000000, 0.000000000000000000 ) ) ;
#10378 = LINE ( 'NONE', #14987, #7492 ) ;
#10379 = ORIENTED_EDGE ( 'NONE', *, *, #7216, .F. ) ;
#10380 = CARTESIAN_POINT ( 'NONE',  ( 82.87092262195501746, 61.16184052528804926, 0.1830206181285179701 ) ) ;
#10381 = ORIENTED_EDGE ( 'NONE', *, *, #18902, .F. ) ;
#10382 = CARTESIAN_POINT ( 'NONE',  ( 229.3257029665984419, 37.51163360410157566, -16.29291827778590118 ) ) ;
#10383 = DIRECTION ( 'NONE',  ( 0.5000000000000052180, -0.8660254037844355990, 0.000000000000000000 ) ) ;
#10384 = AXIS2_PLACEMENT_3D ( 'NONE', #5255, #296, #19382 ) ;
#10385 = DIRECTION ( 'NONE',  ( 1.000000000000000000, 0.000000000000000000, 0.000000000000000000 ) ) ;
#10386 = VECTOR ( 'NONE', #16073, 1000.000000000000114 ) ;
#10387 = CARTESIAN_POINT ( 'NONE',  ( 226.9780240722163001, 41.57793272902847548, -10.22226263383615930 ) ) ;
#10388 = ORIENTED_EDGE ( 'NONE', *, *, #11253, .F. ) ;
#10389 = FACE_OUTER_BOUND ( 'NONE', #11806, .T. ) ;
#10390 = CARTESIAN_POINT ( 'NONE',  ( -17.04169990913787913, 79.99999999999985789, -12.45923801546573095 ) ) ;
#10391 = CARTESIAN_POINT ( 'NONE',  ( 211.6467004136641208, 6.580176515810935989, -25.78004855466132739 ) ) ;
#10392 = CARTESIAN_POINT ( 'NONE',  ( 4.000000000000000000, 5.278424836066145431, -3.047500000000006093 ) ) ;
#10393 = EDGE_LOOP ( 'NONE', ( #3773, #5426, #11201, #6592 ) ) ;
#10394 = ADVANCED_FACE ( 'NONE', ( #18533 ), #20212, .F. ) ;
#10395 = B_SPLINE_CURVE_WITH_KNOTS ( 'NONE', 3,
 ( #5423, #12024, #15222, #16892 ),
 .UNSPECIFIED., .F., .F.,
 ( 4, 4 ),
 ( 7.218489860149274802E-05, 0.0007448356906551951507 ),
 .UNSPECIFIED. ) ;
#10396 = EDGE_CURVE ( 'NONE', #10601, #14228, #4002, .T. ) ;
#10397 = CARTESIAN_POINT ( 'NONE',  ( 219.1657043289025921, 10.92127545031173774, -12.56699194733521097 ) ) ;
#10398 = B_SPLINE_CURVE_WITH_KNOTS ( 'NONE', 3,
 ( #18670, #8593, #4145, #11891 ),
 .UNSPECIFIED., .F., .F.,
 ( 4, 4 ),
 ( 4.014081919079423402E-07, 0.0004524546499717883885 ),
 .UNSPECIFIED. ) ;
#10399 = CARTESIAN_POINT ( 'NONE',  ( 211.2398691629905159, 12.72204434944011986, -24.79563718815145279 ) ) ;
#10400 = AXIS2_PLACEMENT_3D ( 'NONE', #7452, #20599, #18812 ) ;
#10401 = CARTESIAN_POINT ( 'NONE',  ( -27.29860958162435480, 64.25000000000000000, 5.347094680480811490 ) ) ;
#10402 = PRODUCT ( '60-Degree Angle Clamping Handle', '60-Degree Angle Clamping Handle', '', ( #14448 ) ) ;
#10403 = ORIENTED_EDGE ( 'NONE', *, *, #8516, .F. ) ;
#10404 = DIRECTION ( 'NONE',  ( -0.8660254037844357100, -0.5000000000000051070, 0.000000000000000000 ) ) ;
#10406 = DIRECTION ( 'NONE',  ( 0.8660254037844352659, 0.5000000000000056621, 0.000000000000000000 ) ) ;
#10405 = VECTOR ( 'NONE', #18445, 1000.000000000000000 ) ;
#10407 = ADVANCED_FACE ( 'NONE', ( #8875 ), #2527, .F. ) ;
#10408 = FACE_OUTER_BOUND ( 'NONE', #8989, .T. ) ;
#10409 = FACE_BOUND ( 'NONE', #20530, .T. ) ;
#10411 = VERTEX_POINT ( 'NONE', #519 ) ;
#10410 = ORIENTED_EDGE ( 'NONE', *, *, #8777, .T. ) ;
#10412 = ORIENTED_EDGE ( 'NONE', *, *, #2131, .T. ) ;
#10413 = EDGE_LOOP ( 'NONE', ( #11444, #11474, #11373, #19937 ) ) ;
#10414 = DIRECTION ( 'NONE',  ( -0.8660254037844355990, -0.5000000000000054401, 8.343535232742331521E-16 ) ) ;
#10415 = CARTESIAN_POINT ( 'NONE',  ( 227.3277337522544883, 40.97221779530342189, -10.60500809762007179 ) ) ;
#10416 = ADVANCED_FACE ( 'NONE', ( #20009 ), #725, .T. ) ;
#10417 = CARTESIAN_POINT ( 'NONE',  ( 79.36047190431891352, 49.49999999999888445, -13.48535184266127551 ) ) ;
#10418 = AXIS2_PLACEMENT_3D ( 'NONE', #16774, #2255, #18471 ) ;
#10419 = CARTESIAN_POINT ( 'NONE',  ( -29.99999999999966249, 5.000000000000310862, 0.9384178472467484822 ) ) ;
#10420 = SHAPE_REPRESENTATION_RELATIONSHIP ( 'NONE' , 'NONE' ,  #14136, #12645 ) ;
#10421 = DIRECTION ( 'NONE',  ( 0.8404609622712050365, 0.000000000000000000, 0.5418720982834971389 ) ) ;
#10422 = ORIENTED_EDGE ( 'NONE', *, *, #16931, .F. ) ;
#10423 = EDGE_CURVE ( 'NONE', #918, #15282, #2211, .T. ) ;
#10424 =( GEOMETRIC_REPRESENTATION_CONTEXT ( 3 ) GLOBAL_UNCERTAINTY_ASSIGNED_CONTEXT ( ( #898 ) ) GLOBAL_UNIT_ASSIGNED_CONTEXT ( ( #14114, #9619, #3169 ) ) REPRESENTATION_CONTEXT ( 'NONE', 'WORKASPACE' ) );
#10425 = CARTESIAN_POINT ( 'NONE',  ( 81.66740910649770058, 62.54383302279143919, -25.26856822461360608 ) ) ;
#10426 = DIRECTION ( 'NONE',  ( 0.000000000000000000, -0.6846849967427193207, 0.7288391147814602400 ) ) ;
#10427 = ORIENTED_EDGE ( 'NONE', *, *, #16130, .F. ) ;
#10428 = CARTESIAN_POINT ( 'NONE',  ( 58.57586221349259858, 85.50000000000002842, -12.50000000002017231 ) ) ;
#10429 = LINE ( 'NONE', #16913, #5317 ) ;
#10430 = EDGE_CURVE ( 'NONE', #5830, #2244, #8669, .T. ) ;
#10431 = FACE_OUTER_BOUND ( 'NONE', #811, .T. ) ;
#10432 = CARTESIAN_POINT ( 'NONE',  ( 227.9553588074475954, 39.88513931160571957, -14.00000000000005507 ) ) ;
#10433 = CARTESIAN_POINT ( 'NONE',  ( 200.2378745322256464, -0.5219184168523266498, -7.515250618841284869 ) ) ;
#10434 = EDGE_CURVE ( 'NONE', #20411, #9561, #19794, .T. ) ;
#10435 = VECTOR ( 'NONE', #10837, 1000.000000000000227 ) ;
#10436 = ORIENTED_EDGE ( 'NONE', *, *, #15159, .T. ) ;
#10437 = ORIENTED_EDGE ( 'NONE', *, *, #169, .F. ) ;
#10438 = DIRECTION ( 'NONE',  ( 0.5000000000000052180, -0.8660254037844355990, 1.665334536937734318E-16 ) ) ;
#10439 = FACE_OUTER_BOUND ( 'NONE', #2405, .T. ) ;
#10440 = VERTEX_POINT ( 'NONE', #13763 ) ;
#10441 = VERTEX_POINT ( 'NONE', #931 ) ;
#10442 = FACE_OUTER_BOUND ( 'NONE', #20031, .T. ) ;
#10443 = CARTESIAN_POINT ( 'NONE',  ( 209.4659469037960093, 16.35291703476779546, -2.579136038830255107 ) ) ;
#10444 = B_SPLINE_CURVE_WITH_KNOTS ( 'NONE', 3,
 ( #3250, #5042, #14831, #5246 ),
 .UNSPECIFIED., .F., .F.,
 ( 4, 4 ),
 ( 8.982943871858821536E-05, 0.0009438151766972277881 ),
 .UNSPECIFIED. ) ;
#10445 = EDGE_CURVE ( 'NONE', #7341, #8941, #7512, .T. ) ;
#10446 = PLANE ( 'NONE',  #11030 ) ;
#10447 = CARTESIAN_POINT ( 'NONE',  ( -16.71219703957330438, 71.55985624430604730, -4.952210724505382800 ) ) ;
#10448 = AXIS2_PLACEMENT_3D ( 'NONE', #3788, #5056, #2208 ) ;
#10449 = CARTESIAN_POINT ( 'NONE',  ( 78.05328906524978549, 56.09831538232894843, -3.025823995327162841 ) ) ;
#10450 = EDGE_CURVE ( 'NONE', #8387, #2861, #18360, .T. ) ;
#10451 = CARTESIAN_POINT ( 'NONE',  ( 32.39721438298033007, 261.8427481158985302, -5.999999999999973355 ) ) ;
#10452 = CARTESIAN_POINT ( 'NONE',  ( -25.97610854243320588, 50.06551567652685009, -13.91464430999257651 ) ) ;
#10453 = DIRECTION ( 'NONE',  ( 0.000000000000000000, 0.6846849967427193207, -0.7288391147814602400 ) ) ;
#10454 = DIRECTION ( 'NONE',  ( -0.8660254037844370423, -0.5000000000000027756, -1.818545872641207967E-15 ) ) ;
#10455 = CARTESIAN_POINT ( 'NONE',  ( -28.30706676095798713, 52.46230133324129952, 2.217793569358140537 ) ) ;
#10457 = ORIENTED_EDGE ( 'NONE', *, *, #6789, .F. ) ;
#10456 = EDGE_LOOP ( 'NONE', ( #733, #5132 ) ) ;
#10458 = CARTESIAN_POINT ( 'NONE',  ( 203.3234976231973405, 23.93187681866833216, -13.90173226369915405 ) ) ;
#10459 = CARTESIAN_POINT ( 'NONE',  ( 61.48790260083684700, 83.25974565949677242, -18.50556687427830127 ) ) ;
#10460 = EDGE_CURVE ( 'NONE', #3882, #20176, #8773, .T. ) ;
#10461 = ORIENTED_EDGE ( 'NONE', *, *, #20287, .T. ) ;
#10462 = ORIENTED_EDGE ( 'NONE', *, *, #2540, .T. ) ;
#10463 = VECTOR ( 'NONE', #929, 1000.000000000000000 ) ;
#10464 = ORIENTED_EDGE ( 'NONE', *, *, #17147, .T. ) ;
#10465 = LINE ( 'NONE', #8575, #12889 ) ;
#10466 = LINE ( 'NONE', #3909, #7978 ) ;
#10467 = CIRCLE ( 'NONE', #11165, 3.619616396367202782 ) ;
#10468 = ORIENTED_EDGE ( 'NONE', *, *, #6942, .F. ) ;
#10469 = ORIENTED_EDGE ( 'NONE', *, *, #1517, .T. ) ;
#10470 = CARTESIAN_POINT ( 'NONE',  ( 216.3355731942785951, 15.66405044361498788, -16.89203719259520753 ) ) ;
#10471 = VECTOR ( 'NONE', #2515, 1000.000000000000000 ) ;
#10472 = CARTESIAN_POINT ( 'NONE',  ( 81.10655718899290889, 54.43739570252013493, -2.927339837283823520 ) ) ;
#10473 = FACE_OUTER_BOUND ( 'NONE', #3337, .T. ) ;
#10474 = EDGE_LOOP ( 'NONE', ( #10258, #7069, #525, #19855 ) ) ;
#10475 = FACE_OUTER_BOUND ( 'NONE', #20408, .T. ) ;
#10476 = EDGE_LOOP ( 'NONE', ( #17122, #19446, #19658, #12761 ) ) ;
#10477 = FACE_OUTER_BOUND ( 'NONE', #8760, .T. ) ;
#10478 = CARTESIAN_POINT ( 'NONE',  ( 199.6091165883520659, 23.51942873589650773, -14.00000000000005507 ) ) ;
#10479 = DIRECTION ( 'NONE',  ( -0.8660254037843260200, -0.5000000000001951772, 0.000000000000000000 ) ) ;
#10480 = AXIS2_PLACEMENT_3D ( 'NONE', #5315, #368, #19749 ) ;
#10481 = CARTESIAN_POINT ( 'NONE',  ( -27.91449807164519825, 74.13367381892543051, 3.782735275914649087 ) ) ;
#10482 = AXIS2_PLACEMENT_3D ( 'NONE', #1956, #5015, #17964 ) ;
#10483 = DIRECTION ( 'NONE',  ( -0.05035489893517522408, -0.02907241445524020446, -0.9983081582712679536 ) ) ;
#10484 = DIRECTION ( 'NONE',  ( 1.000000000000000000, 0.000000000000000000, 0.000000000000000000 ) ) ;
#10485 = ORIENTED_EDGE ( 'NONE', *, *, #9368, .T. ) ;
#10486 = CARTESIAN_POINT ( 'NONE',  ( 79.38331026022220271, 58.02222229763877692, -1.520680142459543305 ) ) ;
#10487 = ORIENTED_EDGE ( 'NONE', *, *, #9701, .F. ) ;
#10488 = DIRECTION ( 'NONE',  ( 0.2883401610574281571, -0.4994198088140628378, 0.8169698930104470902 ) ) ;
#10489 = CARTESIAN_POINT ( 'NONE',  ( 77.79949723222266300, 55.74148623974197392, -3.361091198315218520 ) ) ;
#10490 = AXIS2_PLACEMENT_3D ( 'NONE', #1928, #1819, #6890 ) ;
#10491 = ADVANCED_FACE ( 'NONE', ( #5365 ), #11966, .F. ) ;
#10492 = MANIFOLD_SOLID_BREP ( 'Hex', #20828 ) ;
#10493 = CARTESIAN_POINT ( 'NONE',  ( 0.000000000000000000, 0.000000000000000000, 0.000000000000000000 ) ) ;
#10494 = TOROIDAL_SURFACE ( 'NONE', #2042, 6.099999999999999645, 0.4000000000000000222 ) ;
#10495 = VECTOR ( 'NONE', #9365, 1000.000000000000114 ) ;
#10496 = DIRECTION ( 'NONE',  ( 0.5999999999999998668, 2.775557561562894309E-16, -0.8000000000000001554 ) ) ;
#10497 = VERTEX_POINT ( 'NONE', #2840 ) ;
#10498 = CARTESIAN_POINT ( 'NONE',  ( 75.02738531498535224, 51.99608617524740595, -12.36235906538899521 ) ) ;
#10499 = CARTESIAN_POINT ( 'NONE',  ( 227.9553588074475670, 39.88513931160575510, -14.00000000000005507 ) ) ;
#10500 = PLANE ( 'NONE',  #18124 ) ;
#10501 = DIRECTION ( 'NONE',  ( 0.5000000000000045519, -0.8660254037844362651, 0.000000000000000000 ) ) ;
#10502 = AXIS2_PLACEMENT_3D ( 'NONE', #3907, #18439, #16848 ) ;
#10503 = ORIENTED_EDGE ( 'NONE', *, *, #5108, .T. ) ;
#10504 = ORIENTED_EDGE ( 'NONE', *, *, #498, .F. ) ;
#10505 = DIRECTION ( 'NONE',  ( 0.1503837331804316335, 0.08682408883346437456, -0.9848077530122086864 ) ) ;
#10506 = AXIS2_PLACEMENT_3D ( 'NONE', #9829, #3374, #14651 ) ;
#10507 = VECTOR ( 'NONE', #17228, 1000.000000000000000 ) ;
#10508 = AXIS2_PLACEMENT_3D ( 'NONE', #19209, #19306, #4580 ) ;
#10509 = CARTESIAN_POINT ( 'NONE',  ( 227.9553588074475954, 39.88513931160571957, -14.00000000000005507 ) ) ;
#10510 = CARTESIAN_POINT ( 'NONE',  ( -27.76586288966045046, 64.25000000000001421, 4.519411796990929098 ) ) ;
#10511 = ORIENTED_EDGE ( 'NONE', *, *, #11959, .F. ) ;
#10512 = AXIS2_PLACEMENT_3D ( 'NONE', #19416, #8169, #1618 ) ;
#10513 = DIRECTION ( 'NONE',  ( -0.2300325188655767683, 0.3984280100682212056, -0.8878852184023763305 ) ) ;
#10514 = CARTESIAN_POINT ( 'NONE',  ( 197.5418782473972499, 4.813505606965178707, -5.993340328401664863 ) ) ;
#10515 = VECTOR ( 'NONE', #18517, 1000.000000000000114 ) ;
#10516 = LINE ( 'NONE', #15331, #400 ) ;
#10517 = CARTESIAN_POINT ( 'NONE',  ( -15.73951718899008512, 80.00000000000179057, -12.49947570859690416 ) ) ;
#10518 = VECTOR ( 'NONE', #1538, 1000.000000000000000 ) ;
#10519 = ADVANCED_FACE ( 'NONE', ( #10347 ), #6205, .T. ) ;
#10521 = ORIENTED_EDGE ( 'NONE', *, *, #7230, .T. ) ;
#10520 = ORIENTED_EDGE ( 'NONE', *, *, #11081, .T. ) ;
#10522 = ORIENTED_EDGE ( 'NONE', *, *, #11477, .T. ) ;
#10523 = ADVANCED_FACE ( 'NONE', ( #4629, #20626, #11096 ), #17569, .T. ) ;
#10524 = LINE ( 'NONE', #2490, #14295 ) ;
#10525 = DIRECTION ( 'NONE',  ( -0.8660254037844380415, -0.5000000000000014433, -0.000000000000000000 ) ) ;
#10526 = CARTESIAN_POINT ( 'NONE',  ( 199.0943133668587564, -1.182153763511707867, -18.09983247376283089 ) ) ;
#10527 = ORIENTED_EDGE ( 'NONE', *, *, #12948, .F. ) ;
#10528 = CIRCLE ( 'NONE', #14968, 11.98469917212512215 ) ;
#10529 = CARTESIAN_POINT ( 'NONE',  ( 215.1214136286681082, 19.61810227076572843, -12.41782726985285557 ) ) ;
#10530 = AXIS2_PLACEMENT_3D ( 'NONE', #2856, #15893, #6009 ) ;
#10531 = LINE ( 'NONE', #3971, #12675 ) ;
#10532 = ORIENTED_EDGE ( 'NONE', *, *, #16178, .F. ) ;
#10533 = VECTOR ( 'NONE', #12578, 999.9999999999998863 ) ;
#10534 = EDGE_CURVE ( 'NONE', #1000, #17941, #1149, .T. ) ;
#10535 = CARTESIAN_POINT ( 'NONE',  ( 82.63287099403851244, 64.35888726086905365, -25.60638951267676688 ) ) ;
#10536 = DIRECTION ( 'NONE',  ( -0.000000000000000000, -0.000000000000000000, 1.000000000000000000 ) ) ;
#10537 = ORIENTED_EDGE ( 'NONE', *, *, #13316, .F. ) ;
#10538 = CYLINDRICAL_SURFACE ( 'NONE', #14276, 12.47473710546057646 ) ;
#10539 = CARTESIAN_POINT ( 'NONE',  ( 218.3788871517383257, 37.95555635890104185, -12.27491058351074393 ) ) ;
#10540 = ADVANCED_FACE ( 'NONE', ( #15991 ), #5890, .T. ) ;
#10541 = CYLINDRICAL_SURFACE ( 'NONE', #1016, 12.47473710546057646 ) ;
#10542 = LINE ( 'NONE', #17028, #18966 ) ;
#10543 = AXIS2_PLACEMENT_3D ( 'NONE', #12353, #17010, #14161 ) ;
#10544 = DIRECTION ( 'NONE',  ( 0.5171545105027588463, 0.2985792958514013051, 0.8021231927550364071 ) ) ;
#10545 = VERTEX_POINT ( 'NONE', #10663 ) ;
#10546 = ORIENTED_EDGE ( 'NONE', *, *, #1755, .T. ) ;
#10547 = AXIS2_PLACEMENT_3D ( 'NONE', #5710, #19929, #648 ) ;
#10548 = DIRECTION ( 'NONE',  ( -0.8660254037844368202, -0.5000000000000032196, 0.000000000000000000 ) ) ;
#10550 = CARTESIAN_POINT ( 'NONE',  ( 177.1791022559528983, 56.75747545832872731, -14.00000000000006395 ) ) ;
#10549 = VECTOR ( 'NONE', #8077, 1000.000000000000000 ) ;
#10551 = EDGE_CURVE ( 'NONE', #3195, #18441, #271, .T. ) ;
#10552 = ORIENTED_EDGE ( 'NONE', *, *, #7559, .T. ) ;
#10553 = B_SPLINE_CURVE_WITH_KNOTS ( 'NONE', 3,
 ( #19973, #2389, #12541, #9330, #5439, #8742, #15239, #15829, #692, #7147, #13636, #8847, #5550, #15346, #17933, #6358, #225, #3395 ),
 .UNSPECIFIED., .F., .F.,
 ( 4, 2, 2, 2, 2, 2, 2, 2, 4 ),
 ( 0.02406572584676644130, 0.02716336196282548646, 0.03026099807888454549, 0.03180981613691406806, 0.03335863419494358717, 0.03413304322395834672, 0.03490745225297310628, 0.03568186128198786583, 0.03645627031100262538 ),
 .UNSPECIFIED. ) ;
#10554 = VERTEX_POINT ( 'NONE', #7594 ) ;
#10555 = ORIENTED_EDGE ( 'NONE', *, *, #18145, .T. ) ;
#10556 = DIRECTION ( 'NONE',  ( 0.5000000000000041078, -0.8660254037844363761, 0.000000000000000000 ) ) ;
#10557 = CARTESIAN_POINT ( 'NONE',  ( 80.21122190583011502, 51.84991952600655196, -5.522095467871776187 ) ) ;
#10558 = CARTESIAN_POINT ( 'NONE',  ( 30.00000000000000000, -10.00000000000000000, 15.00000000000000000 ) ) ;
#10559 = DIRECTION ( 'NONE',  ( 0.000000000000000000, -1.000000000000000000, 0.000000000000000000 ) ) ;
#10560 = CARTESIAN_POINT ( 'NONE',  ( -18.30887993796372726, 70.93184341055301445, -4.446547635559178424 ) ) ;
#10561 = EDGE_CURVE ( 'NONE', #491, #6727, #2633, .T. ) ;
#10562 = EDGE_CURVE ( 'NONE', #13651, #19586, #12390, .T. ) ;
#10563 = CARTESIAN_POINT ( 'NONE',  ( 204.9818247258934321, 9.640009970873842704, -2.036337243043272238 ) ) ;
#10564 = VECTOR ( 'NONE', #6564, 1000.000000000000227 ) ;
#10565 = VECTOR ( 'NONE', #5473, 1000.000000000000114 ) ;
#10566 = CARTESIAN_POINT ( 'NONE',  ( 105.9489074543212013, 187.9071680446163555, 11.00000000000001066 ) ) ;
#10567 = CARTESIAN_POINT ( 'NONE',  ( -19.40591372560455596, 45.47726231970822397, -12.03202924821253283 ) ) ;
#10568 = FACE_OUTER_BOUND ( 'NONE', #8469, .T. ) ;
#10569 = EDGE_CURVE ( 'NONE', #142, #10186, #18984, .T. ) ;
#10570 = FACE_OUTER_BOUND ( 'NONE', #17617, .T. ) ;
#10571 = SHAPE_REPRESENTATION ( 'Rear Drill Bit Retaining Pin', ( #18233 ), #14867 ) ;
#10572 = FACE_OUTER_BOUND ( 'NONE', #15407, .T. ) ;
#10574 = ORIENTED_EDGE ( 'NONE', *, *, #20279, .T. ) ;
#10573 = VERTEX_POINT ( 'NONE', #6098 ) ;
#10575 = CARTESIAN_POINT ( 'NONE',  ( 202.6368254117890046, 24.70800346662761626, -12.57697892669095019 ) ) ;
#10576 = CARTESIAN_POINT ( 'NONE',  ( 62.19646603496936166, 78.41412544775637627, -13.18179411983555660 ) ) ;
#10577 = ORIENTED_EDGE ( 'NONE', *, *, #3555, .F. ) ;
#10578 = ORIENTED_EDGE ( 'NONE', *, *, #9220, .T. ) ;
#10579 = ORIENTED_EDGE ( 'NONE', *, *, #20804, .F. ) ;
#10580 = CARTESIAN_POINT ( 'NONE',  ( 218.9914638623158396, 11.07829152179047760, -11.13829696442610029 ) ) ;
#10581 = CARTESIAN_POINT ( 'NONE',  ( -0.7537384908010169582, 50.28366646829528719, -9.578226701023302425 ) ) ;
#10582 = DIRECTION ( 'NONE',  ( 0.8679903670753312817, 0.4965810333313504521, 0.000000000000000000 ) ) ;
#10583 = EDGE_CURVE ( 'NONE', #18856, #9864, #9869, .T. ) ;
#10584 = VERTEX_POINT ( 'NONE', #19056 ) ;
#10585 = ORIENTED_EDGE ( 'NONE', *, *, #10314, .F. ) ;
#10586 = CARTESIAN_POINT ( 'NONE',  ( 218.3177700343719039, 36.57793272902843995, -10.22226263383615574 ) ) ;
#10587 = EDGE_CURVE ( 'NONE', #16648, #19116, #17214, .T. ) ;
#10588 = DIRECTION ( 'NONE',  ( -0.8660254037844355990, -0.5000000000000055511, 0.000000000000000000 ) ) ;
#10589 = CARTESIAN_POINT ( 'NONE',  ( -20.89897948556633978, 16.09941697557071905, 0.9999999999999991118 ) ) ;
#10590 = ADVANCED_FACE ( 'NONE', ( #17464 ), #2111, .T. ) ;
#10591 = PRODUCT ( 'socket head cap screw_iso_ISO 4762 M10 x 70 - 32N', 'socket head cap screw_iso_ISO 4762 M10 x 70 - 32N', '', ( #15926 ) ) ;
#10592 = DIRECTION ( 'NONE',  ( 0.8660254037844370423, 0.5000000000000026645, -0.000000000000000000 ) ) ;
#10593 = CARTESIAN_POINT ( 'NONE',  ( 217.2468988696282963, 38.43273599472488655, -15.14518239232894636 ) ) ;
#10595 = FACE_OUTER_BOUND ( 'NONE', #7536, .T. ) ;
#10594 = ADVANCED_BREP_SHAPE_REPRESENTATION ( '', ( #3258, #18233 ), #20586 ) ;
#10596 = LINE ( 'NONE', #5821, #9566 ) ;
#10597 = AXIS2_PLACEMENT_3D ( 'NONE', #19557, #5035, #11511 ) ;
#10598 = CARTESIAN_POINT ( 'NONE',  ( 199.1738290307970374, -1.136245373532171588, -9.972943347741736630 ) ) ;
#10599 = LINE ( 'NONE', #4352, #20434 ) ;
#10600 = DIRECTION ( 'NONE',  ( -0.05035489893516262305, -0.02907241445523293250, 0.9983081582712687307 ) ) ;
#10601 = VERTEX_POINT ( 'NONE', #14401 ) ;
#10602 = CARTESIAN_POINT ( 'NONE',  ( 79.96260520138829975, 55.97221593644851367, -3.110880007782513168 ) ) ;
#10603 = VERTEX_POINT ( 'NONE', #1456 ) ;
#10604 = ORIENTED_EDGE ( 'NONE', *, *, #18111, .T. ) ;
#10605 = DIRECTION ( 'NONE',  ( -0.8660254037844357100, -0.5000000000000051070, 0.000000000000000000 ) ) ;
#10606 = DIRECTION ( 'NONE',  ( 0.5000000000000029976, -0.8660254037844370423, 0.000000000000000000 ) ) ;
#10607 = PRODUCT_CONTEXT ( 'NONE', #18665, 'mechanical' ) ;
#10608 = AXIS2_PLACEMENT_3D ( 'NONE', #16985, #8814, #10610 ) ;
#10609 = CIRCLE ( 'NONE', #1158, 12.47473710546057823 ) ;
#10610 = DIRECTION ( 'NONE',  ( 0.5000000000000057732, -0.8660254037844353769, 0.000000000000000000 ) ) ;
#10611 = ORIENTED_EDGE ( 'NONE', *, *, #11304, .F. ) ;
#10612 = DIRECTION ( 'NONE',  ( -0.5000000000000045519, 0.8660254037844360431, 0.000000000000000000 ) ) ;
#10613 = DIRECTION ( 'NONE',  ( -1.000000000000000000, -0.000000000000000000, -0.000000000000000000 ) ) ;
#10614 = FACE_OUTER_BOUND ( 'NONE', #7241, .T. ) ;
#10615 = LINE ( 'NONE', #20471, #8114 ) ;
#10616 = FACE_OUTER_BOUND ( 'NONE', #15749, .T. ) ;
#10617 = DIRECTION ( 'NONE',  ( 0.8660254037844372643, 0.5000000000000027756, -0.000000000000000000 ) ) ;
#10618 = ADVANCED_FACE ( 'NONE', ( #1767 ), #6486, .T. ) ;
#10619 = PLANE ( 'NONE',  #20910 ) ;
#10620 = ORIENTED_EDGE ( 'NONE', *, *, #2139, .F. ) ;
#10621 = DIRECTION ( 'NONE',  ( -0.8660254037844380415, -0.5000000000000014433, -0.000000000000000000 ) ) ;
#10622 = DIRECTION ( 'NONE',  ( 0.000000000000000000, -6.938893903907177533E-18, -1.000000000000000000 ) ) ;
#10623 = CARTESIAN_POINT ( 'NONE',  ( 220.3643805408902381, 35.16445410620250556, -10.10863206319042362 ) ) ;
#10624 = CARTESIAN_POINT ( 'NONE',  ( 4.000000000000000000, -1.759474945355379072, 3.047500000000001652 ) ) ;
#10626 = VERTEX_POINT ( 'NONE', #272 ) ;
#10625 = EDGE_LOOP ( 'NONE', ( #18882, #7443, #10427, #16394, #17262 ) ) ;
#10627 = ORIENTED_EDGE ( 'NONE', *, *, #13810, .F. ) ;
#10628 = CARTESIAN_POINT ( 'NONE',  ( 159.9952905943348469, 46.83639716978957068, 0.9999999999999386047 ) ) ;
#10629 = LINE ( 'NONE', #5959, #1750 ) ;
#10630 = VERTEX_POINT ( 'NONE', #9593 ) ;
#10631 = PRODUCT_DEFINITION_CONTEXT ( 'detailed design', #19600, 'design' ) ;
#10632 = EDGE_CURVE ( 'NONE', #951, #3051, #15340, .T. ) ;
#10633 = AXIS2_PLACEMENT_3D ( 'NONE', #7250, #20187, #687 ) ;
#10634 = CARTESIAN_POINT ( 'NONE',  ( 205.5965122587965084, 9.994899983462953941, -14.00000000000005507 ) ) ;
#10635 = MANIFOLD_SOLID_BREP ( 'Cut-Extrude8', #5927 ) ;
#10636 = CARTESIAN_POINT ( 'NONE',  ( 198.0735972701637024, -1.389238810292188875, -14.00000000000005507 ) ) ;
#10637 = EDGE_CURVE ( 'NONE', #17637, #2259, #6512, .T. ) ;
#10638 = ORIENTED_EDGE ( 'NONE', *, *, #1211, .F. ) ;
#10639 = EDGE_CURVE ( 'NONE', #14308, #14580, #8002, .T. ) ;
#10640 = CARTESIAN_POINT ( 'NONE',  ( 159.9952905943347901, 46.83639716978955647, -22.00000000000007816 ) ) ;
#10641 = CYLINDRICAL_SURFACE ( 'NONE', #253, 15.00000000000000000 ) ;
#10642 = LINE ( 'NONE', #17126, #3705 ) ;
#10643 = DIRECTION ( 'NONE',  ( -0.5000000000000037748, 0.8660254037844364872, 0.000000000000000000 ) ) ;
#10644 = CARTESIAN_POINT ( 'NONE',  ( 177.1791022559528983, 56.75747545832873442, -29.00000000000007105 ) ) ;
#10645 = ORIENTED_EDGE ( 'NONE', *, *, #2540, .F. ) ;
#10646 = ORIENTED_EDGE ( 'NONE', *, *, #1906, .F. ) ;
#10647 = FACE_BOUND ( 'NONE', #12326, .T. ) ;
#10648 = ORIENTED_EDGE ( 'NONE', *, *, #7773, .F. ) ;
#10649 = CIRCLE ( 'NONE', #11729, 3.309499999999999886 ) ;
#10650 = CARTESIAN_POINT ( 'NONE',  ( 44.21948262095328630, 217.3659788670219370, 44.53282986889900030 ) ) ;
#10651 = DIRECTION ( 'NONE',  ( 0.8660254037844378194, 0.5000000000000013323, 0.000000000000000000 ) ) ;
#10652 = CARTESIAN_POINT ( 'NONE',  ( 200.4167038695724443, 7.004336215593725434, -24.38552490958304020 ) ) ;
#10653 = DIRECTION ( 'NONE',  ( -0.8660254037844362651, -0.5000000000000042188, 6.872020471724002955E-17 ) ) ;
#10654 = CARTESIAN_POINT ( 'NONE',  ( -20.31374355284814825, 65.74999999999995737, -2.528164662410434804 ) ) ;
#10655 = VERTEX_POINT ( 'NONE', #8101 ) ;
#10656 = ADVANCED_FACE ( 'NONE', ( #6407 ), #9997, .F. ) ;
#10657 = EDGE_LOOP ( 'NONE', ( #9640, #3254, #2363, #19728 ) ) ;
#10658 = ORIENTED_EDGE ( 'NONE', *, *, #11302, .F. ) ;
#10659 = CLOSED_SHELL ( 'NONE', ( #2005, #2772, #11755, #9441, #14116, #2423, #5907, #18948, #10540, #13296, #15791, #7618, #9152, #17917, #20296, #7569 ) ) ;
#10660 = DIRECTION ( 'NONE',  ( -0.8660254037844360431, -0.5000000000000045519, -4.336808689942049784E-16 ) ) ;
#10661 = EDGE_CURVE ( 'NONE', #15787, #9257, #172, .T. ) ;
#10662 = AXIS2_PLACEMENT_3D ( 'NONE', #15710, #8311, #12620 ) ;
#10663 = CARTESIAN_POINT ( 'NONE',  ( 210.1178786253386193, 12.07426281049857408, -2.551678190571530891 ) ) ;
#10664 = CARTESIAN_POINT ( 'NONE',  ( -14.07807032132161318, 50.45729534307898234, -16.17568974221241618 ) ) ;
#10665 = CARTESIAN_POINT ( 'NONE',  ( 228.5339464938061553, 38.23003690969649426, -10.60379488450933394 ) ) ;
#10666 = VECTOR ( 'NONE', #12649, 1000.000000000000000 ) ;
#10667 = FACE_OUTER_BOUND ( 'NONE', #4878, .T. ) ;
#10668 = CARTESIAN_POINT ( 'NONE',  ( -28.49367486532711524, 49.92396641514135069, 0.4641840246318328922 ) ) ;
#10670 = ORIENTED_EDGE ( 'NONE', *, *, #11565, .T. ) ;
#10669 = ORIENTED_EDGE ( 'NONE', *, *, #7428, .F. ) ;
#10671 = DIRECTION ( 'NONE',  ( -0.3841106397986888688, 0.6652991438591145945, -0.6401843996644803747 ) ) ;
#10672 = CARTESIAN_POINT ( 'NONE',  ( 208.6933310212059496, 11.60583922538805268, -2.363289276295987840 ) ) ;
#10673 = CARTESIAN_POINT ( 'NONE',  ( -3.513138912839586681, 80.00000000007391066, -0.6469719004569252085 ) ) ;
#10674 = ORIENTED_EDGE ( 'NONE', *, *, #6765, .F. ) ;
#10675 = ORIENTED_EDGE ( 'NONE', *, *, #18062, .T. ) ;
#10676 = EDGE_CURVE ( 'NONE', #16137, #13251, #13213, .T. ) ;
#10677 = FACE_OUTER_BOUND ( 'NONE', #10476, .T. ) ;
#10678 = CARTESIAN_POINT ( 'NONE',  ( 205.8264633344831225, 9.596613037118636669, -14.00000000000005507 ) ) ;
#10679 = CARTESIAN_POINT ( 'NONE',  ( -2.305711553939125746, 50.03762982245009283, -11.32446199378746421 ) ) ;
#10680 = CARTESIAN_POINT ( 'NONE',  ( -33.99999999999997868, 65.74999999999995737, -2.528164662410434804 ) ) ;
#10681 = ORIENTED_EDGE ( 'NONE', *, *, #12127, .F. ) ;
#10682 = ORIENTED_EDGE ( 'NONE', *, *, #20645, .F. ) ;
#10683 = VECTOR ( 'NONE', #5616, 1000.000000000000000 ) ;
#10684 = VERTEX_POINT ( 'NONE', #17987 ) ;
#10685 = LINE ( 'NONE', #2653, #8366 ) ;
#10686 = CIRCLE ( 'NONE', #17488, 5.000000000000000888 ) ;
#10687 = EDGE_CURVE ( 'NONE', #13380, #7589, #13011, .T. ) ;
#10688 = DIRECTION ( 'NONE',  ( 0.5000000000000054401, -0.8660254037844354880, 2.220446049250312834E-16 ) ) ;
#10689 = CARTESIAN_POINT ( 'NONE',  ( 220.3709088428545613, 34.50527358010378265, -10.54439633573330859 ) ) ;
#10690 = FACE_OUTER_BOUND ( 'NONE', #6889, .T. ) ;
#10691 = ADVANCED_FACE ( 'NONE', ( #3453 ), #5136, .F. ) ;
#10692 = ORIENTED_EDGE ( 'NONE', *, *, #4187, .T. ) ;
#10693 = CARTESIAN_POINT ( 'NONE',  ( 229.0957782906355078, 37.58340574881690088, -16.68717795561669703 ) ) ;
#10694 = FACE_OUTER_BOUND ( 'NONE', #2623, .T. ) ;
#10695 = CARTESIAN_POINT ( 'NONE',  ( 229.8865181528416315, 36.54027320787180599, -14.55761806292095706 ) ) ;
#10696 = AXIS2_PLACEMENT_3D ( 'NONE', #2253, #5103, #8708 ) ;
#10697 = EDGE_CURVE ( 'NONE', #5922, #513, #19055, .T. ) ;
#10698 = ORIENTED_EDGE ( 'NONE', *, *, #861, .T. ) ;
#10699 = CARTESIAN_POINT ( 'NONE',  ( -28.94934366394663883, 73.64887869707766299, -0.2211343278575746418 ) ) ;
#10700 = LINE ( 'NONE', #10804, #10970 ) ;
#10701 = CARTESIAN_POINT ( 'NONE',  ( 227.9553588074475670, 39.88513931160575510, -14.00000000000005507 ) ) ;
#10702 = AXIS2_PLACEMENT_3D ( 'NONE', #7064, #13547, #5460 ) ;
#10703 = ORIENTED_EDGE ( 'NONE', *, *, #16178, .T. ) ;
#10704 = AXIS2_PLACEMENT_3D ( 'NONE', #2397, #4197, #20405 ) ;
#10705 = CARTESIAN_POINT ( 'NONE',  ( 80.60135456229210149, 66.45530591845690083, 0.4295846759676194559 ) ) ;
#10706 = EDGE_CURVE ( 'NONE', #2569, #18021, #2406, .T. ) ;
#10707 = ORIENTED_EDGE ( 'NONE', *, *, #10182, .F. ) ;
#10708 = EDGE_CURVE ( 'NONE', #5066, #15695, #5159, .T. ) ;
#10709 = ORIENTED_EDGE ( 'NONE', *, *, #17717, .F. ) ;
#10710 = CARTESIAN_POINT ( 'NONE',  ( 208.8107687779841228, 4.427644383670616079, -14.00000000000005507 ) ) ;
#10711 = CARTESIAN_POINT ( 'NONE',  ( 78.05328906524978549, 56.09831538232894843, -3.025823995327163729 ) ) ;
#10712 = MANIFOLD_SOLID_BREP ( 'Chamfer1', #15451 ) ;
#10713 =( NAMED_UNIT ( * ) SI_UNIT ( $, .STERADIAN. ) SOLID_ANGLE_UNIT ( ) );
#10714 = EDGE_CURVE ( 'NONE', #5457, #18365, #403, .T. ) ;
#10715 = DIRECTION ( 'NONE',  ( 0.000000000000000000, -1.000000000000000000, 6.938893903907177533E-18 ) ) ;
#10716 = ORIENTED_EDGE ( 'NONE', *, *, #8492, .T. ) ;
#10717 = AXIS2_PLACEMENT_3D ( 'NONE', #8042, #14552, #12953 ) ;
#10718 = DIRECTION ( 'NONE',  ( -0.000000000000000000, -1.000000000000000000, -0.000000000000000000 ) ) ;
#10719 = CARTESIAN_POINT ( 'NONE',  ( 201.0721825858487364, 0.7325896531374328502, -4.915515517929136990 ) ) ;
#10720 = CARTESIAN_POINT ( 'NONE',  ( -29.99999999999999645, 5.000000000000000000, 30.00000000000000000 ) ) ;
#10721 = DIRECTION ( 'NONE',  ( -0.8660254037844360431, -0.5000000000000044409, 5.976026924694052093E-17 ) ) ;
#10722 = DIRECTION ( 'NONE',  ( -0.8660254037844361541, -0.5000000000000044409, 5.976026924694052093E-17 ) ) ;
#10723 = EDGE_CURVE ( 'NONE', #12475, #15862, #18224, .T. ) ;
#10724 = DIRECTION ( 'NONE',  ( 0.000000000000000000, 0.000000000000000000, 1.000000000000000000 ) ) ;
#10725 = CARTESIAN_POINT ( 'NONE',  ( 159.9952905943348469, 46.83639716978957068, 0.9999999999999386047 ) ) ;
#10726 = FACE_OUTER_BOUND ( 'NONE', #13680, .T. ) ;
#10727 = ORIENTED_EDGE ( 'NONE', *, *, #742, .T. ) ;
#10728 = CARTESIAN_POINT ( 'NONE',  ( 220.2180084519553134, 35.41797800104779270, -14.00000000000005507 ) ) ;
#10729 = VECTOR ( 'NONE', #19917, 1000.000000000000000 ) ;
#10730 = LINE ( 'NONE', #17210, #19688 ) ;
#10731 = CARTESIAN_POINT ( 'NONE',  ( -15.73952097860949273, 79.99999999999998579, -12.49895143242785345 ) ) ;
#10732 = AXIS2_PLACEMENT_3D ( 'NONE', #20453, #18561, #15401 ) ;
#10734 = ORIENTED_EDGE ( 'NONE', *, *, #15653, .F. ) ;
#10733 = ORIENTED_EDGE ( 'NONE', *, *, #2799, .F. ) ;
#10735 = CARTESIAN_POINT ( 'NONE',  ( -15.99999999999999289, 10.09941697557069418, 12.50000000000000000 ) ) ;
#10736 = CARTESIAN_POINT ( 'NONE',  ( 200.8894739819445192, 11.40128808463920329, -25.34310559273323804 ) ) ;
#10737 = EDGE_LOOP ( 'NONE', ( #17425, #11777, #7449, #6247 ) ) ;
#10738 = DIRECTION ( 'NONE',  ( -0.5000000000000051070, 0.8660254037844359321, -0.000000000000000000 ) ) ;
#10739 = CARTESIAN_POINT ( 'NONE',  ( 218.3356494533592240, 38.67831942470078843, -15.02729838650890315 ) ) ;
#10740 = ORIENTED_EDGE ( 'NONE', *, *, #11597, .F. ) ;
#10741 = DIRECTION ( 'NONE',  ( 0.1005394128318207458, 0.05804645706261939847, 0.9932383577419421350 ) ) ;
#10742 = ORIENTED_EDGE ( 'NONE', *, *, #4409, .T. ) ;
#10743 = CIRCLE ( 'NONE', #19546, 4.057500000000029416 ) ;
#10744 = LINE ( 'NONE', #14278, #3120 ) ;
#10745 = DIRECTION ( 'NONE',  ( 0.000000000000000000, 0.000000000000000000, 1.000000000000000000 ) ) ;
#10746 = AXIS2_PLACEMENT_3D ( 'NONE', #16468, #3330, #11702 ) ;
#10747 = ORIENTED_EDGE ( 'NONE', *, *, #17793, .F. ) ;
#10748 = DIRECTION ( 'NONE',  ( 0.8660254037844370423, 0.5000000000000026645, -0.000000000000000000 ) ) ;
#10749 = CARTESIAN_POINT ( 'NONE',  ( 199.8291677591948314, 21.40379373188257972, -1.545471579934816875 ) ) ;
#10750 = DIRECTION ( 'NONE',  ( -1.000000000000000000, -0.000000000000000000, -0.000000000000000000 ) ) ;
#10751 = DIRECTION ( 'NONE',  ( -0.5000000000000045519, 0.8660254037844361541, 0.000000000000000000 ) ) ;
#10752 = CARTESIAN_POINT ( 'NONE',  ( 93.10604617319987142, 25.69196698708779536, -12.49999999999999822 ) ) ;
#10753 = ORIENTED_EDGE ( 'NONE', *, *, #9622, .T. ) ;
#10754 = ORIENTED_EDGE ( 'NONE', *, *, #12917, .T. ) ;
#10755 = DIRECTION ( 'NONE',  ( -0.8660254037844378194, -0.5000000000000013323, -0.000000000000000000 ) ) ;
#10756 = ORIENTED_EDGE ( 'NONE', *, *, #9073, .T. ) ;
#10757 = ORIENTED_EDGE ( 'NONE', *, *, #19628, .F. ) ;
#10758 = VERTEX_POINT ( 'NONE', #20204 ) ;
#10759 = CIRCLE ( 'NONE', #20251, 0.4000000000000001887 ) ;
#10760 = CARTESIAN_POINT ( 'NONE',  ( -20.83678142705256064, 13.78956489930263452, 11.52651691409252521 ) ) ;
#10761 = LINE ( 'NONE', #8964, #3423 ) ;
#10762 = CARTESIAN_POINT ( 'NONE',  ( 227.9553588074475954, 39.88513931160571957, -14.00000000000005507 ) ) ;
#10763 = AXIS2_PLACEMENT_3D ( 'NONE', #12342, #4167, #15532 ) ;
#10764 = DIRECTION ( 'NONE',  ( 1.000000000000000000, 0.000000000000000000, 0.000000000000000000 ) ) ;
#10765 = EDGE_CURVE ( 'NONE', #18457, #17954, #16925, .T. ) ;
#10766 = CARTESIAN_POINT ( 'NONE',  ( 209.3909370991932519, 3.422763374394458769, -14.00000000000005507 ) ) ;
#10767 = ORIENTED_EDGE ( 'NONE', *, *, #7183, .T. ) ;
#10768 = ORIENTED_EDGE ( 'NONE', *, *, #11932, .T. ) ;
#10769 = FACE_OUTER_BOUND ( 'NONE', #2670, .T. ) ;
#10770 = B_SPLINE_CURVE_WITH_KNOTS ( 'NONE', 3,
 ( #11831, #16493, #9803, #14720, #1974, #14824, #17888, #388, #19665, #19872, #3655, #18291, #6840, #3765, #10217, #8538, #15039, #16711, #14923, #4935, #13324, #174, #497, #19452, #2189, #19771, #6514, #5237, #11728, #8641, #18190, #6936 ),
 .UNSPECIFIED., .F., .F.,
 ( 4, 2, 2, 2, 2, 2, 2, 2, 2, 2, 2, 2, 2, 2, 2, 4 ),
 ( -0.0002012768826452384079, 0.001195388216070833671, 0.002592053314786905722, 0.005385383512219049824, 0.008178713709651194361, 0.009575378808367264460, 0.01097204390708333629, 0.01376537410451547823, 0.01516203920323155353, 0.01655870430194762363, 0.01795536940066369894, 0.01865370195002173312, 0.01935203449937976730, 0.02074869959809586342, 0.02144703214745389760, 0.02214536469681193526 ),
 .UNSPECIFIED. ) ;
#10771 = VECTOR ( 'NONE', #17408, 1000.000000000000114 ) ;
#10772 = CARTESIAN_POINT ( 'NONE',  ( -29.99999999999999645, -10.00000000000000000, 0.000000000000000000 ) ) ;
#10773 = CARTESIAN_POINT ( 'NONE',  ( -22.54565399147047344, 45.14475518768605866, -10.65478537919073254 ) ) ;
#10774 = DIRECTION ( 'NONE',  ( -0.5000000000000049960, 0.8660254037844358210, -0.000000000000000000 ) ) ;
#10775 = LINE ( 'NONE', #12701, #20646 ) ;
#10776 = EDGE_CURVE ( 'NONE', #3810, #15949, #11266, .T. ) ;
#10777 = CARTESIAN_POINT ( 'NONE',  ( -28.15715448389819997, 53.81647424313067773, 2.930203991123683238 ) ) ;
#10779 = VERTEX_POINT ( 'NONE', #20104 ) ;
#10778 = ORIENTED_EDGE ( 'NONE', *, *, #7891, .F. ) ;
#10780 = CARTESIAN_POINT ( 'NONE',  ( 196.0270608673617687, 8.593972564023673044, -4.392917125964746816 ) ) ;
#10781 = LINE ( 'NONE', #4330, #13245 ) ;
#10782 =( NAMED_UNIT ( * ) PLANE_ANGLE_UNIT ( ) SI_UNIT ( $, .RADIAN. ) );
#10783 = VERTEX_POINT ( 'NONE', #7062 ) ;
#10784 = ORIENTED_EDGE ( 'NONE', *, *, #10160, .T. ) ;
#10785 = FACE_OUTER_BOUND ( 'NONE', #8729, .T. ) ;
#10786 = CARTESIAN_POINT ( 'NONE',  ( 41.50490953756720813, 222.0677573683055925, -8.999999999999971578 ) ) ;
#10787 = CARTESIAN_POINT ( 'NONE',  ( -17.58792505510971083, 50.46559566222132531, -16.20915785584423929 ) ) ;
#10788 = FACE_OUTER_BOUND ( 'NONE', #9013, .T. ) ;
#10789 = ORIENTED_EDGE ( 'NONE', *, *, #18858, .T. ) ;
#10790 = EDGE_CURVE ( 'NONE', #19064, #17011, #17486, .T. ) ;
#10791 = VECTOR ( 'NONE', #2341, 999.9999999999998863 ) ;
#10792 = VERTEX_POINT ( 'NONE', #11955 ) ;
#10793 = EDGE_CURVE ( 'NONE', #4941, #16061, #13983, .T. ) ;
#10794 = LINE ( 'NONE', #14219, #17527 ) ;
#10795 =( GEOMETRIC_REPRESENTATION_CONTEXT ( 3 ) GLOBAL_UNCERTAINTY_ASSIGNED_CONTEXT ( ( #4903 ) ) GLOBAL_UNIT_ASSIGNED_CONTEXT ( ( #18366, #9018, #10713 ) ) REPRESENTATION_CONTEXT ( 'NONE', 'WORKASPACE' ) );
#10796 = DIRECTION ( 'NONE',  ( -0.4330127018922105275, -0.2499999999999986955, 0.8660254037844433705 ) ) ;
#10797 = PLANE ( 'NONE',  #7565 ) ;
#10798 = CARTESIAN_POINT ( 'NONE',  ( 214.7634125556922129, 15.28741233751021156, -19.29168348739315775 ) ) ;
#10799 = EDGE_CURVE ( 'NONE', #17847, #245, #11659, .T. ) ;
#10800 = DIRECTION ( 'NONE',  ( -0.8660254037844357100, -0.5000000000000049960, 0.000000000000000000 ) ) ;
#10801 = CARTESIAN_POINT ( 'NONE',  ( 197.6726970570908293, -1.230104231997219300, -14.01558723443171850 ) ) ;
#10802 = DIRECTION ( 'NONE',  ( -0.000000000000000000, -1.000000000000000000, -0.000000000000000000 ) ) ;
#10803 = CARTESIAN_POINT ( 'NONE',  ( -28.65583546987735275, 66.09831342192320847, 2.470462955490114965 ) ) ;
#10804 = CARTESIAN_POINT ( 'NONE',  ( 205.6766695652311512, 24.77985047368454019, -4.003039906354141308 ) ) ;
#10805 = LINE ( 'NONE', #11129, #80 ) ;
#10806 = AXIS2_PLACEMENT_3D ( 'NONE', #18531, #8872, #14084 ) ;
#10807 = ORIENTED_EDGE ( 'NONE', *, *, #15838, .F. ) ;
#10809 = EDGE_CURVE ( 'NONE', #6449, #14979, #18935, .T. ) ;
#10808 = CARTESIAN_POINT ( 'NONE',  ( 81.33834232799965491, 66.66102642021321856, 0.6137031208531950055 ) ) ;
#10810 = VERTEX_POINT ( 'NONE', #10650 ) ;
#10811 = VERTEX_POINT ( 'NONE', #10985 ) ;
#10812 = DIRECTION ( 'NONE',  ( 0.000000000000000000, 0.9982500481053682151, 0.05913409725048478921 ) ) ;
#10813 = DIRECTION ( 'NONE',  ( -0.8660254037844354880, -0.5000000000000055511, 0.000000000000000000 ) ) ;
#10814 = VECTOR ( 'NONE', #20796, 1000.000000000000000 ) ;
#10815 = EDGE_CURVE ( 'NONE', #7001, #4766, #3063, .T. ) ;
#10816 = APPLICATION_PROTOCOL_DEFINITION ( 'draft international standard', 'automotive_design', 1998, #16771 ) ;
#10817 = CARTESIAN_POINT ( 'NONE',  ( 219.8530131173444033, 35.43232009577518227, -17.56803216753788988 ) ) ;
#10818 = VERTEX_POINT ( 'NONE', #9168 ) ;
#10819 = DIRECTION ( 'NONE',  ( 0.000000000000000000, 1.000000000000000000, 1.155257860108281416E-16 ) ) ;
#10820 = VECTOR ( 'NONE', #1641, 1000.000000000000114 ) ;
#10821 = CARTESIAN_POINT ( 'NONE',  ( 204.3420759002525529, 1.847643347786420698, -26.10173121575770594 ) ) ;
#10822 = DIRECTION ( 'NONE',  ( 0.000000000000000000, -1.000000000000000000, 0.000000000000000000 ) ) ;
#10823 = CARTESIAN_POINT ( 'NONE',  ( -25.99999999999999645, 9.999999999999994671, -7.500000000000000000 ) ) ;
#10824 = EDGE_CURVE ( 'NONE', #7471, #7703, #6087, .T. ) ;
#10825 = CIRCLE ( 'NONE', #5069, 11.94520687646042667 ) ;
#10826 = EDGE_CURVE ( 'NONE', #15665, #7763, #14340, .T. ) ;
#10827 = CARTESIAN_POINT ( 'NONE',  ( 219.2080768649571496, 11.20335309717537520, -15.43274561385901400 ) ) ;
#10828 = CARTESIAN_POINT ( 'NONE',  ( 215.9040783327276358, 15.94597603093701466, -15.40420431385954281 ) ) ;
#10829 = PLANE ( 'NONE',  #16964 ) ;
#10830 = PLANE ( 'NONE',  #3997 ) ;
#10831 = VERTEX_POINT ( 'NONE', #1339 ) ;
#10833 = EDGE_CURVE ( 'NONE', #13343, #3954, #7582, .T. ) ;
#10832 = DIRECTION ( 'NONE',  ( 1.000000000000000000, 0.000000000000000000, -1.445602896647336205E-16 ) ) ;
#10834 = LINE ( 'NONE', #9033, #6756 ) ;
#10835 = CARTESIAN_POINT ( 'NONE',  ( 188.4825312237924777, 14.85281007377110640, -15.43274561385865695 ) ) ;
#10836 = VECTOR ( 'NONE', #9953, 1000.000000000000114 ) ;
#10837 = DIRECTION ( 'NONE',  ( -0.8660254037844370423, -0.5000000000000026645, 0.000000000000000000 ) ) ;
#10839 = ORIENTED_EDGE ( 'NONE', *, *, #18975, .F. ) ;
#10838 = ORIENTED_EDGE ( 'NONE', *, *, #13188, .F. ) ;
#10840 = CIRCLE ( 'NONE', #12886, 11.98469917212512215 ) ;
#10841 = CARTESIAN_POINT ( 'NONE',  ( 213.9878548032869503, 18.96364177778961491, -15.39542905462748656 ) ) ;
#10842 = EDGE_LOOP ( 'NONE', ( #13308, #17321, #15049, #4727, #891 ) ) ;
#10843 = UNCERTAINTY_MEASURE_WITH_UNIT (LENGTH_MEASURE( 1.000000000000000082E-05 ), #20398, 'distance_accuracy_value', 'NONE');
#10844 = EDGE_CURVE ( 'NONE', #20933, #4158, #17029, .T. ) ;
#10845 = AXIS2_PLACEMENT_3D ( 'NONE', #16951, #8786, #11980 ) ;
#10846 = LINE ( 'NONE', #2813, #19499 ) ;
#10847 = LINE ( 'NONE', #4290, #262 ) ;
#10848 = DIRECTION ( 'NONE',  ( -0.9795788631971408256, 0.000000000000000000, -0.2010603162670278610 ) ) ;
#10849 = CIRCLE ( 'NONE', #11422, 11.98469917212512215 ) ;
#10850 = ORIENTED_EDGE ( 'NONE', *, *, #20916, .F. ) ;
#10851 = VERTEX_POINT ( 'NONE', #15867 ) ;
#10852 = CARTESIAN_POINT ( 'NONE',  ( 214.9988779556950078, 8.000350883196837515, -23.57241037536588735 ) ) ;
#10853 = AXIS2_PLACEMENT_3D ( 'NONE', #7215, #15510, #16976 ) ;
#10854 =( NAMED_UNIT ( * ) SI_UNIT ( $, .STERADIAN. ) SOLID_ANGLE_UNIT ( ) );
#10855 = AXIS2_PLACEMENT_3D ( 'NONE', #1358, #20634, #2744 ) ;
#10856 = ORIENTED_EDGE ( 'NONE', *, *, #10676, .T. ) ;
#10857 = CARTESIAN_POINT ( 'NONE',  ( 208.9119903699346708, 11.37804290162847209, -2.044871543907030631 ) ) ;
#10858 = CARTESIAN_POINT ( 'NONE',  ( 226.1594288993896953, 42.99578115919451449, -13.55260094074449739 ) ) ;
#10859 = B_SPLINE_CURVE_WITH_KNOTS ( 'NONE', 3,
 ( #11124, #3172, #2970, #16020 ),
 .UNSPECIFIED., .F., .F.,
 ( 4, 4 ),
 ( 4.013058786232072053E-07, 0.0004524545476585053799 ),
 .UNSPECIFIED. ) ;
#10860 = AXIS2_PLACEMENT_3D ( 'NONE', #13026, #9713, #6422 ) ;
#10861 = LINE ( 'NONE', #3128, #13883 ) ;
#10862 = CARTESIAN_POINT ( 'NONE',  ( 34.99529059433363898, 263.3427481158985302, -22.00000000000000355 ) ) ;
#10863 = B_SPLINE_CURVE_WITH_KNOTS ( 'NONE', 3,
 ( #17436, #7455, #13950, #20492 ),
 .UNSPECIFIED., .F., .F.,
 ( 4, 4 ),
 ( 6.919709117646055681E-07, 0.0006733427629651237561 ),
 .UNSPECIFIED. ) ;
#10864 = ORIENTED_EDGE ( 'NONE', *, *, #16540, .T. ) ;
#10865 = EDGE_LOOP ( 'NONE', ( #17762, #16206, #9943, #20820, #16150 ) ) ;
#10866 = LINE ( 'NONE', #6193, #10533 ) ;
#10867 = VECTOR ( 'NONE', #18706, 1000.000000000000227 ) ;
#10868 = ORIENTED_EDGE ( 'NONE', *, *, #6555, .F. ) ;
#10869 = EDGE_LOOP ( 'NONE', ( #14309, #4606, #5721, #5377 ) ) ;
#10870 = CARTESIAN_POINT ( 'NONE',  ( -15.99999999999999289, 10.09941697557069418, 12.50000000000000000 ) ) ;
#10871 = CARTESIAN_POINT ( 'NONE',  ( 184.9952905943350459, 3.535126980567751431, -22.00000000000009948 ) ) ;
#10872 = VECTOR ( 'NONE', #4375, 1000.000000000000114 ) ;
#10873 = DIRECTION ( 'NONE',  ( -1.000000000000000000, -0.000000000000000000, -0.000000000000000000 ) ) ;
#10874 = CIRCLE ( 'NONE', #17655, 4.400000000000000355 ) ;
#10875 = DIRECTION ( 'NONE',  ( -0.5000000000000054401, 0.8660254037844354880, -0.000000000000000000 ) ) ;
#10876 = LINE ( 'NONE', #20516, #14849 ) ;
#10877 = CIRCLE ( 'NONE', #11903, 5.999999999999998224 ) ;
#10878 = ORIENTED_EDGE ( 'NONE', *, *, #15607, .T. ) ;
#10879 = DIRECTION ( 'NONE',  ( 0.5000000000000051070, -0.8660254037844359321, 0.000000000000000000 ) ) ;
#10880 = AXIS2_PLACEMENT_3D ( 'NONE', #18177, #1961, #2069 ) ;
#10881 = DIRECTION ( 'NONE',  ( 0.000000000000000000, 0.000000000000000000, 1.000000000000000000 ) ) ;
#10882 = CARTESIAN_POINT ( 'NONE',  ( -19.64325535697088654, 49.51382188615453117, -11.96543228433093198 ) ) ;
#10883 = CARTESIAN_POINT ( 'NONE',  ( 228.0528179502890964, 39.71633512454245363, -17.56803216753791475 ) ) ;
#10884 = VECTOR ( 'NONE', #446, 1000.000000000000114 ) ;
#10885 = CONICAL_SURFACE ( 'NONE', #3775, 13.07248899748297433, 0.6693469023067423196 ) ;
#10886 = DIRECTION ( 'NONE',  ( 0.000000000000000000, 0.000000000000000000, -1.000000000000000000 ) ) ;
#10887 = VECTOR ( 'NONE', #18347, 1000.000000000000114 ) ;
#10888 = DIRECTION ( 'NONE',  ( -0.5000000000000049960, 0.8660254037844358210, -0.000000000000000000 ) ) ;
#10889 = ADVANCED_FACE ( 'NONE', ( #7787 ), #14292, .F. ) ;
#10891 = VERTEX_POINT ( 'NONE', #3029 ) ;
#10890 = ORIENTED_EDGE ( 'NONE', *, *, #18317, .T. ) ;
#10892 = CARTESIAN_POINT ( 'NONE',  ( 207.0274154277438754, 3.398024846849156511, -2.233628351993186101 ) ) ;
#10893 = FACE_OUTER_BOUND ( 'NONE', #1423, .T. ) ;
#10894 = DIRECTION ( 'NONE',  ( 0.5000000000000052180, -0.8660254037844355990, 1.665334536937734564E-16 ) ) ;
#10895 = VERTEX_POINT ( 'NONE', #7477 ) ;
#10896 = VERTEX_POINT ( 'NONE', #1026 ) ;
#10897 = ORIENTED_EDGE ( 'NONE', *, *, #13306, .F. ) ;
#10898 = CARTESIAN_POINT ( 'NONE',  ( 218.7758640552229679, 37.26797219263381322, -16.70098974528087155 ) ) ;
#10899 = CARTESIAN_POINT ( 'NONE',  ( 218.6737414447757715, 35.96137216016707328, -10.64970491435233235 ) ) ;
#10900 = CARTESIAN_POINT ( 'NONE',  ( -22.23810050820787865, 50.28853357967717130, -15.44648544901684950 ) ) ;
#10901 = FACE_OUTER_BOUND ( 'NONE', #17472, .T. ) ;
#10902 = ORIENTED_EDGE ( 'NONE', *, *, #9926, .T. ) ;
#10903 = AXIS2_PLACEMENT_3D ( 'NONE', #17230, #10750, #13959 ) ;
#10904 = ORIENTED_EDGE ( 'NONE', *, *, #20392, .F. ) ;
#10905 = CARTESIAN_POINT ( 'NONE',  ( 206.9147384664715901, 10.75597823931698294, -11.08174281168198227 ) ) ;
#10906 = ORIENTED_EDGE ( 'NONE', *, *, #1363, .T. ) ;
#10907 = VECTOR ( 'NONE', #12425, 1000.000000000000227 ) ;
#10908 = AXIS2_PLACEMENT_3D ( 'NONE', #2711, #12569, #10968 ) ;
#10909 = B_SPLINE_CURVE_WITH_KNOTS ( 'NONE', 3,
 ( #2990, #14349, #6983, #8685 ),
 .UNSPECIFIED., .F., .F.,
 ( 4, 4 ),
 ( 2.844611917656723886E-07, 0.0004523377029716364435 ),
 .UNSPECIFIED. ) ;
#10911 = EDGE_CURVE ( 'NONE', #8365, #17033, #15683, .T. ) ;
#10910 = DIRECTION ( 'NONE',  ( 0.5171545105027589573, 0.2985792958514010831, 0.8021231927550364071 ) ) ;
#10912 = AXIS2_PLACEMENT_3D ( 'NONE', #13451, #19899, #13347 ) ;
#10913 = DIRECTION ( 'NONE',  ( 0.000000000000000000, -0.8108848540793835991, 0.5852057359806522863 ) ) ;
#10914 = CARTESIAN_POINT ( 'NONE',  ( 226.7538876070129277, 41.96614847458961606, -11.35524774226743361 ) ) ;
#10915 = CARTESIAN_POINT ( 'NONE',  ( 77.98781333307499608, 70.07958826284888687, -25.26506956498398893 ) ) ;
#10916 = CARTESIAN_POINT ( 'NONE',  ( 207.4656388362384973, 11.07404071609857077, -17.01204567730803063 ) ) ;
#10917 = DIRECTION ( 'NONE',  ( 0.8660254037844355990, 0.5000000000000054401, 5.284238980736809733E-15 ) ) ;
#10918 = DIRECTION ( 'NONE',  ( -0.5000000000000047740, 0.8660254037844358210, 0.000000000000000000 ) ) ;
#10919 = ADVANCED_FACE ( 'NONE', ( #7366 ), #7527, .F. ) ;
#10920 = VERTEX_POINT ( 'NONE', #4203 ) ;
#10921 = DIRECTION ( 'NONE',  ( -1.000000000000000000, 0.000000000000000000, 0.000000000000000000 ) ) ;
#10922 = CARTESIAN_POINT ( 'NONE',  ( 202.0139385235187035, 1.276312697262135920, -4.003039906353937916 ) ) ;
#10923 = DIRECTION ( 'NONE',  ( 0.000000000000000000, 0.8847993391852124745, 0.4659722409944731525 ) ) ;
#10924 = EDGE_CURVE ( 'NONE', #11617, #1231, #5983, .T. ) ;
#10925 = ORIENTED_EDGE ( 'NONE', *, *, #10430, .F. ) ;
#10926 = CARTESIAN_POINT ( 'NONE',  ( 80.30982465549199389, 65.77076383589957231, 0.4787884790452578976 ) ) ;
#10927 = AXIS2_PLACEMENT_3D ( 'NONE', #17667, #5020, #19439 ) ;
#10928 = ORIENTED_EDGE ( 'NONE', *, *, #13, .T. ) ;
#10929 = B_SPLINE_CURVE_WITH_KNOTS ( 'NONE', 3,
 ( #4923, #4721, #3235, #17767 ),
 .UNSPECIFIED., .F., .F.,
 ( 4, 4 ),
 ( 3.242053695154241001E-07, 0.0008543099433544477624 ),
 .UNSPECIFIED. ) ;
#10930 = ORIENTED_EDGE ( 'NONE', *, *, #10274, .F. ) ;
#10931 = CARTESIAN_POINT ( 'NONE',  ( -3.074305435089455862, 72.33610889977832414, 0.5975377147116670562 ) ) ;
#10932 = CARTESIAN_POINT ( 'NONE',  ( 219.0871984830704662, 10.36074384021052985, -12.62839849932177394 ) ) ;
#10933 = APPLICATION_PROTOCOL_DEFINITION ( 'draft international standard', 'automotive_design', 1998, #14637 ) ;
#10934 = CARTESIAN_POINT ( 'NONE',  ( 226.1821525240497976, 42.95642268675138808, -13.56204498775453970 ) ) ;
#10935 = ORIENTED_EDGE ( 'NONE', *, *, #7040, .T. ) ;
#10936 = PRODUCT_DEFINITION ( 'UNKNOWN', '', #18249, #14271 ) ;
#10937 = DIRECTION ( 'NONE',  ( 1.000000000000000000, -0.000000000000000000, -0.000000000000000000 ) ) ;
#10938 = DIRECTION ( 'NONE',  ( 0.5000000000000054401, -0.8660254037844354880, -2.220446049250312834E-16 ) ) ;
#10939 = VECTOR ( 'NONE', #16324, 1000.000000000000000 ) ;
#10940 = CARTESIAN_POINT ( 'NONE',  ( 199.2144802262915846, 21.04890371929339921, -14.00000000000005507 ) ) ;
#10941 = CARTESIAN_POINT ( 'NONE',  ( 208.8577037357181894, 4.346350652224124644, -14.00000000000005507 ) ) ;
#10942 = ADVANCED_FACE ( 'NONE', ( #17353 ), #3438, .T. ) ;
#10943 = LINE ( 'NONE', #7751, #10666 ) ;
#10944 = LINE ( 'NONE', #9124, #19687 ) ;
#10945 = ADVANCED_FACE ( 'NONE', ( #11609 ), #11295, .F. ) ;
#10946 = FACE_OUTER_BOUND ( 'NONE', #9323, .T. ) ;
#10947 = CARTESIAN_POINT ( 'NONE',  ( 206.2937561296588456, 1.095629421411969950, -14.00000000000005507 ) ) ;
#10948 = DIRECTION ( 'NONE',  ( -0.5000000000000008882, 0.8660254037844381525, 0.000000000000000000 ) ) ;
#10949 = EDGE_LOOP ( 'NONE', ( #17950, #5351, #4306, #3355 ) ) ;
#10950 = DIRECTION ( 'NONE',  ( -1.000000000000000000, -0.000000000000000000, -0.000000000000000000 ) ) ;
#10951 = EDGE_CURVE ( 'NONE', #11581, #6296, #103, .T. ) ;
#10952 = CARTESIAN_POINT ( 'NONE',  ( -4.693238136585347497, 66.39265442260773398, 5.329868606387891283 ) ) ;
#10953 = EDGE_CURVE ( 'NONE', #4965, #17368, #1788, .T. ) ;
#10954 = CARTESIAN_POINT ( 'NONE',  ( 202.1791022559531541, 13.45620526910691694, -14.00000000000008527 ) ) ;
#10955 = CARTESIAN_POINT ( 'NONE',  ( 199.2144802262915846, 21.04890371929339921, -14.00000000000005507 ) ) ;
#10956 = CARTESIAN_POINT ( 'NONE',  ( -28.62307079896444506, 76.35052269458219598, -2.692414605357462687 ) ) ;
#10957 = VECTOR ( 'NONE', #6307, 1000.000000000000000 ) ;
#10959 = ORIENTED_EDGE ( 'NONE', *, *, #3089, .T. ) ;
#10958 = ORIENTED_EDGE ( 'NONE', *, *, #1533, .T. ) ;
#10960 = EDGE_CURVE ( 'NONE', #11736, #15521, #12145, .T. ) ;
#10961 = CARTESIAN_POINT ( 'NONE',  ( -13.77473633848136636, 10.61006857860113151, 12.30409397790407233 ) ) ;
#10962 = FILL_AREA_STYLE ('',( #1525 ) ) ;
#10963 = ORIENTED_EDGE ( 'NONE', *, *, #20937, .T. ) ;
#10964 = CARTESIAN_POINT ( 'NONE',  ( 228.8412418162020003, 38.35074493088110614, -10.52303454827241502 ) ) ;
#10965 = CARTESIAN_POINT ( 'NONE',  ( 45.00000000000000000, 5.000000000000000000, 15.00000000000000000 ) ) ;
#10966 = CARTESIAN_POINT ( 'NONE',  ( 205.5965122587965084, 9.994899983462953941, -14.00000000000005507 ) ) ;
#10967 = EDGE_CURVE ( 'NONE', #6104, #15417, #11947, .T. ) ;
#10968 = DIRECTION ( 'NONE',  ( 0.000000000000000000, 0.000000000000000000, -1.000000000000000000 ) ) ;
#10969 = VECTOR ( 'NONE', #7422, 1000.000000000000114 ) ;
#10970 = VECTOR ( 'NONE', #4249, 1000.000000000000227 ) ;
#10971 =( NAMED_UNIT ( * ) PLANE_ANGLE_UNIT ( ) SI_UNIT ( $, .RADIAN. ) );
#10972 = ORIENTED_EDGE ( 'NONE', *, *, #10967, .F. ) ;
#10973 = CARTESIAN_POINT ( 'NONE',  ( 208.8107687779841228, 4.427644383670616079, -14.00000000000005507 ) ) ;
#10974 = CARTESIAN_POINT ( 'NONE',  ( 221.8782118065657869, 32.54242143996614089, -11.94979443502200844 ) ) ;
#10975 = EDGE_CURVE ( 'NONE', #385, #19414, #19542, .T. ) ;
#10976 = EDGE_CURVE ( 'NONE', #1421, #8955, #62, .T. ) ;
#10977 = PLANE ( 'NONE',  #6753 ) ;
#10978 = CARTESIAN_POINT ( 'NONE',  ( 214.9514471701782270, 8.488172945287894677, -4.138477629886256004 ) ) ;
#10979 = ORIENTED_EDGE ( 'NONE', *, *, #16868, .T. ) ;
#10980 = FACE_OUTER_BOUND ( 'NONE', #5398, .T. ) ;
#10981 = ADVANCED_FACE ( 'NONE', ( #1548 ), #9841, .T. ) ;
#10982 = ORIENTED_EDGE ( 'NONE', *, *, #7076, .T. ) ;
#10983 = ORIENTED_EDGE ( 'NONE', *, *, #8464, .T. ) ;
#10984 = EDGE_CURVE ( 'NONE', #14638, #14727, #14809, .T. ) ;
#10985 = CARTESIAN_POINT ( 'NONE',  ( 228.0559782506801980, 39.71086132369779165, -17.61401795338991505 ) ) ;
#10986 = CARTESIAN_POINT ( 'NONE',  ( 79.37186041290443939, 49.53105059404756361, -11.54859855717600325 ) ) ;
#10987 = CARTESIAN_POINT ( 'NONE',  ( 204.6045052031513478, 24.16083609062223303, -3.188775577416895324 ) ) ;
#10988 = AXIS2_PLACEMENT_3D ( 'NONE', #70, #9989, #5130 ) ;
#10989 = DIRECTION ( 'NONE',  ( 0.8660254037844355990, 0.5000000000000054401, 0.000000000000000000 ) ) ;
#10990 =( NAMED_UNIT ( * ) SI_UNIT ( $, .STERADIAN. ) SOLID_ANGLE_UNIT ( ) );
#10991 = ADVANCED_FACE ( 'NONE', ( #19646 ), #13643, .T. ) ;
#10992 = ORIENTED_EDGE ( 'NONE', *, *, #18100, .T. ) ;
#10993 = DIRECTION ( 'NONE',  ( -0.9170191824714420958, 0.000000000000000000, -0.3988431007042845255 ) ) ;
#10994 = B_SPLINE_CURVE_WITH_KNOTS ( 'NONE', 3,
 ( #6455, #13058, #17826, #15827, #12959, #11144, #17409, #7855, #19407, #17729, #1300, #3193, #20682, #4886, #1504, #16140, #3295, #9646, #6356, #2888, #14249, #6155, #16043, #1607, #7952, #11353, #12851, #14354, #8048, #19305, #3097, #9745 ),
 .UNSPECIFIED., .F., .F.,
 ( 4, 2, 2, 2, 2, 2, 2, 2, 2, 2, 2, 2, 2, 2, 2, 4 ),
 ( 5.204170427930421283E-18, 0.0004893630623245339177, 0.0009787261246490626312, 0.001468089186973591236, 0.001957452249298120058, 0.002936178373947171197, 0.003425541436271701320, 0.003914904498596230575, 0.004404267560920760265, 0.004893630623245289954, 0.005382993685569818776, 0.005872356747894348465, 0.006361719810218879022, 0.006851082872543407844, 0.007340445934867937533, 0.007829808997192468090 ),
 .UNSPECIFIED. ) ;
#10995 = ORIENTED_EDGE ( 'NONE', *, *, #1507, .T. ) ;
#10996 = FILL_AREA_STYLE_COLOUR ( '', #16017 ) ;
#10997 = CARTESIAN_POINT ( 'NONE',  ( -4.694333320860708980, 51.54365109033042103, -5.670238636117967523 ) ) ;
#10998 = CARTESIAN_POINT ( 'NONE',  ( 115.7566812678108050, 36.45991617951909092, -12.49999999999999822 ) ) ;
#10999 = CIRCLE ( 'NONE', #18783, 11.98469917212512215 ) ;
#11000 = EDGE_CURVE ( 'NONE', #20919, #3253, #1793, .T. ) ;
#11001 = LINE ( 'NONE', #7700, #4048 ) ;
#11002 = CARTESIAN_POINT ( 'NONE',  ( -16.77277943456198628, 45.63508326896292999, -12.50000000000000178 ) ) ;
#11004 = ORIENTED_EDGE ( 'NONE', *, *, #18599, .T. ) ;
#11003 = ORIENTED_EDGE ( 'NONE', *, *, #4847, .F. ) ;
#11005 = CARTESIAN_POINT ( 'NONE',  ( 218.8798129321970976, 10.24100973658777924, -16.73990883341947367 ) ) ;
#11006 = CARTESIAN_POINT ( 'NONE',  ( 157.3972143829815309, 45.33639716978955647, -6.000000000000052403 ) ) ;
#11007 = CARTESIAN_POINT ( 'NONE',  ( 0.7085851579124478050, 78.02673419564928281, -5.061054382486330105 ) ) ;
#11008 = EDGE_LOOP ( 'NONE', ( #13575, #10469, #9529, #12250 ) ) ;
#11009 = ORIENTED_EDGE ( 'NONE', *, *, #9549, .T. ) ;
#11010 = CARTESIAN_POINT ( 'NONE',  ( 220.5205374755283572, 32.76262760368710047, -17.47639052459127740 ) ) ;
#11011 = CARTESIAN_POINT ( 'NONE',  ( 229.0176887497488849, 38.04512987713822270, -11.06956603356930202 ) ) ;
#11012 = CARTESIAN_POINT ( 'NONE',  ( 1.349294741687074861, 52.07539629968670170, -4.877430129159401773 ) ) ;
#11013 = DIRECTION ( 'NONE',  ( -1.000000000000000000, 0.000000000000000000, 0.000000000000000000 ) ) ;
#11014 = EDGE_LOOP ( 'NONE', ( #6837, #5798, #946, #9768 ) ) ;
#11015 = ORIENTED_EDGE ( 'NONE', *, *, #2917, .F. ) ;
#11016 = PLANE ( 'NONE',  #11758 ) ;
#11017 = SHAPE_REPRESENTATION_RELATIONSHIP ( 'NONE' , 'NONE' ,  #16277, #6793 ) ;
#11018 = LINE ( 'NONE', #1654, #3188 ) ;
#11019 = ADVANCED_FACE ( 'NONE', ( #15336 ), #16797, .F. ) ;
#11020 = VECTOR ( 'NONE', #2134, 1000.000000000000000 ) ;
#11021 = CARTESIAN_POINT ( 'NONE',  ( 225.6488786369508830, 42.90061426249287990, -15.02729838650890493 ) ) ;
#11022 = CARTESIAN_POINT ( 'NONE',  ( 63.75189850252981216, 73.93268399900620125, -21.96684734925903726 ) ) ;
#11023 = CARTESIAN_POINT ( 'NONE',  ( 220.3379369467334925, 35.21025575481678516, -17.89498551959673023 ) ) ;
#11024 = CARTESIAN_POINT ( 'NONE',  ( -27.29860958162435480, 65.74999999999997158, 5.347094680480812379 ) ) ;
#11025 = CARTESIAN_POINT ( 'NONE',  ( 220.7506168395117356, 33.87762484391836892, -10.80501622924635186 ) ) ;
#11026 = CARTESIAN_POINT ( 'NONE',  ( 226.7369255887865904, 41.99552755195625764, -11.32356490392471393 ) ) ;
#11027 = CARTESIAN_POINT ( 'NONE',  ( 27.33334827330880756, 65.75000000000001421, 2.147472525011945521 ) ) ;
#11028 = CARTESIAN_POINT ( 'NONE',  ( 43.85427444295667954, 167.9985379866523942, 11.00000000000001243 ) ) ;
#11029 = EDGE_LOOP ( 'NONE', ( #8324, #16089, #612, #18808 ) ) ;
#11030 = AXIS2_PLACEMENT_3D ( 'NONE', #3888, #2411, #8867 ) ;
#11031 = CARTESIAN_POINT ( 'NONE',  ( 77.50103995547023317, 68.94704969384721949, -0.06791703117014312452 ) ) ;
#11032 = EDGE_CURVE ( 'NONE', #3882, #5656, #3540, .T. ) ;
#11033 = VERTEX_POINT ( 'NONE', #13626 ) ;
#11034 = VERTEX_POINT ( 'NONE', #18276 ) ;
#11035 = CARTESIAN_POINT ( 'NONE',  ( 1.441635642453537702, 75.56468634061762657, -1.801359935164346115 ) ) ;
#11036 = DIRECTION ( 'NONE',  ( 0.000000000000000000, 0.000000000000000000, -1.000000000000000000 ) ) ;
#11037 = CARTESIAN_POINT ( 'NONE',  ( 221.9593540118165151, 32.19590095186362788, -14.99046307270432621 ) ) ;
#11038 = ORIENTED_EDGE ( 'NONE', *, *, #14210, .F. ) ;
#11039 = CARTESIAN_POINT ( 'NONE',  ( 1.500000000000001332, 0.000000000000000000, 0.000000000000000000 ) ) ;
#11040 = ORIENTED_EDGE ( 'NONE', *, *, #12868, .F. ) ;
#11041 = CARTESIAN_POINT ( 'NONE',  ( 211.5616548979095626, 6.788689316162965781, -2.044871543907030631 ) ) ;
#11042 = EDGE_CURVE ( 'NONE', #2725, #9686, #3135, .T. ) ;
#11043 = CARTESIAN_POINT ( 'NONE',  ( 227.5312376355471145, 39.64027283883993391, -14.00000000000005507 ) ) ;
#11044 = CARTESIAN_POINT ( 'NONE',  ( 228.6455928494450234, 37.71015299068947257, -17.20332536629375753 ) ) ;
#11045 = CARTESIAN_POINT ( 'NONE',  ( 0.5040958584341809212, 58.95372983808996992, 1.249471100433037885 ) ) ;
#11046 = EDGE_CURVE ( 'NONE', #9600, #16336, #12131, .T. ) ;
#11047 = VECTOR ( 'NONE', #2520, 1000.000000000000000 ) ;
#11048 = ORIENTED_EDGE ( 'NONE', *, *, #10583, .F. ) ;
#11049 = DIRECTION ( 'NONE',  ( 0.5000000000000057732, -0.8660254037844352659, 4.857225732735059864E-17 ) ) ;
#11050 = LINE ( 'NONE', #4584, #2811 ) ;
#11051 = AXIS2_PLACEMENT_3D ( 'NONE', #5166, #18219, #18017 ) ;
#11052 = CYLINDRICAL_SURFACE ( 'NONE', #13320, 3.902363844300889451 ) ;
#11053 = DIRECTION ( 'NONE',  ( -0.8660254037844370423, -0.5000000000000026645, 0.000000000000000000 ) ) ;
#11054 = VERTEX_POINT ( 'NONE', #2379 ) ;
#11055 = DIRECTION ( 'NONE',  ( 0.000000000000000000, 0.000000000000000000, -1.000000000000000000 ) ) ;
#11056 = CARTESIAN_POINT ( 'NONE',  ( 37.85427444295662269, 178.3908428320656299, 11.00000000000001243 ) ) ;
#11057 = EDGE_CURVE ( 'NONE', #10810, #19247, #16477, .T. ) ;
#11058 = FACE_OUTER_BOUND ( 'NONE', #17587, .T. ) ;
#11059 = CONICAL_SURFACE ( 'NONE', #17496, 3.309499999999999886, 0.7853981633974501664 ) ;
#11060 = CARTESIAN_POINT ( 'NONE',  ( -29.23300298503555439, 76.74099499729592821, -3.129240771529778975 ) ) ;
#11062 = ORIENTED_EDGE ( 'NONE', *, *, #13309, .F. ) ;
#11061 = ORIENTED_EDGE ( 'NONE', *, *, #15108, .F. ) ;
#11063 = CIRCLE ( 'NONE', #8690, 15.00000000000000000 ) ;
#11064 = CARTESIAN_POINT ( 'NONE',  ( 30.00000000000000000, 0.000000000000000000, 15.00000000000000000 ) ) ;
#11065 = EDGE_CURVE ( 'NONE', #14019, #12002, #8168, .T. ) ;
#11066 = CARTESIAN_POINT ( 'NONE',  ( -33.44237801383309261, 75.57646748667876579, -1.814718499151628084 ) ) ;
#11067 = VERTEX_POINT ( 'NONE', #5542 ) ;
#11068 = EDGE_CURVE ( 'NONE', #6425, #2244, #17998, .T. ) ;
#11069 = DIRECTION ( 'NONE',  ( 0.5000000000000051070, -0.8660254037844359321, 0.000000000000000000 ) ) ;
#11070 = ORIENTED_EDGE ( 'NONE', *, *, #17893, .F. ) ;
#11071 = LINE ( 'NONE', #5865, #10205 ) ;
#11072 = EDGE_CURVE ( 'NONE', #15381, #1893, #14908, .T. ) ;
#11073 = ORIENTED_EDGE ( 'NONE', *, *, #18599, .F. ) ;
#11074 = DIRECTION ( 'NONE',  ( -0.9679941405060923376, 0.000000000000000000, -0.2509727952306220478 ) ) ;
#11075 = VECTOR ( 'NONE', #16337, 1000.000000000000227 ) ;
#11076 = DIRECTION ( 'NONE',  ( 0.8660254037844370423, 0.5000000000000026645, -0.000000000000000000 ) ) ;
#11077 = DIRECTION ( 'NONE',  ( -0.8660254037844360431, -0.5000000000000044409, 5.976026924694052093E-17 ) ) ;
#11078 = CARTESIAN_POINT ( 'NONE',  ( 216.3417993343409194, 15.66764510725598214, -11.13829696442610029 ) ) ;
#11079 = ORIENTED_EDGE ( 'NONE', *, *, #9912, .F. ) ;
#11080 = FACE_OUTER_BOUND ( 'NONE', #17131, .T. ) ;
#11081 = EDGE_CURVE ( 'NONE', #3522, #2297, #375, .T. ) ;
#11082 = EDGE_LOOP ( 'NONE', ( #11837, #3264, #14971, #14342, #19068 ) ) ;
#11083 = ORIENTED_EDGE ( 'NONE', *, *, #13309, .T. ) ;
#11084 = CARTESIAN_POINT ( 'NONE',  ( -19.31141590166239652, 11.33920243900448455, 12.05575761655145861 ) ) ;
#11085 = DIRECTION ( 'NONE',  ( 0.000000000000000000, 0.000000000000000000, -1.000000000000000000 ) ) ;
#11086 = DIRECTION ( 'NONE',  ( 0.5000000000000049960, -0.8660254037844358210, 0.000000000000000000 ) ) ;
#11087 = ADVANCED_FACE ( 'NONE', ( #18389 ), #10304, .T. ) ;
#11088 = CYLINDRICAL_SURFACE ( 'NONE', #16789, 4.999999999999989342 ) ;
#11089 = AXIS2_PLACEMENT_3D ( 'NONE', #4750, #15704, #1372 ) ;
#11090 = VERTEX_POINT ( 'NONE', #5428 ) ;
#11091 = CIRCLE ( 'NONE', #17193, 5.000000000000002665 ) ;
#11092 = CARTESIAN_POINT ( 'NONE',  ( 212.1124805811015790, 13.40286946702044979, -23.87887634647646351 ) ) ;
#11093 = EDGE_CURVE ( 'NONE', #16219, #19586, #12030, .T. ) ;
#11094 = EDGE_CURVE ( 'NONE', #11673, #6716, #9984, .T. ) ;
#11095 = ORIENTED_EDGE ( 'NONE', *, *, #14596, .T. ) ;
#11096 = FACE_BOUND ( 'NONE', #17794, .T. ) ;
#11097 = CARTESIAN_POINT ( 'NONE',  ( -8.542481363097889968, 50.20976409724571710, -15.00415514080579271 ) ) ;
#11098 = CARTESIAN_POINT ( 'NONE',  ( 208.0983737146324870, 5.661548828456886895, -14.00000000000005507 ) ) ;
#11099 = LINE ( 'NONE', #20428, #6080 ) ;
#11100 = DIRECTION ( 'NONE',  ( -1.000000000000000000, -0.000000000000000000, -0.000000000000000000 ) ) ;
#11101 = COLOUR_RGB ( '',0.7921568627450980005, 0.8196078431372548767, 0.9333333333333333481 ) ;
#11103 = ORIENTED_EDGE ( 'NONE', *, *, #10723, .F. ) ;
#11102 = EDGE_LOOP ( 'NONE', ( #6056, #12600, #20941, #3881, #4223, #19754 ) ) ;
#11104 = PLANE ( 'NONE',  #19323 ) ;
#11105 = CARTESIAN_POINT ( 'NONE',  ( -33.99999999999997868, 65.74999999999995737, -2.528164662410434804 ) ) ;
#11106 = ADVANCED_FACE ( 'NONE', ( #13408 ), #10202, .F. ) ;
#11107 = VECTOR ( 'NONE', #5011, 1000.000000000000114 ) ;
#11108 =( LENGTH_UNIT ( ) NAMED_UNIT ( * ) SI_UNIT ( .MILLI., .METRE. ) );
#11109 = ORIENTED_EDGE ( 'NONE', *, *, #16314, .F. ) ;
#11110 = ORIENTED_EDGE ( 'NONE', *, *, #11057, .F. ) ;
#11111 = ORIENTED_EDGE ( 'NONE', *, *, #5754, .F. ) ;
#11112 = DIRECTION ( 'NONE',  ( 0.5000000000000041078, -0.8660254037844363761, 0.000000000000000000 ) ) ;
#11113 = CARTESIAN_POINT ( 'NONE',  ( 30.10683012259193703, -24.14213562373095456, -4.999999999999997335 ) ) ;
#11114 = DIRECTION ( 'NONE',  ( 0.000000000000000000, 0.000000000000000000, 1.000000000000000000 ) ) ;
#11115 = CYLINDRICAL_SURFACE ( 'NONE', #5622, 3.902363844300889451 ) ;
#11116 = ORIENTED_EDGE ( 'NONE', *, *, #14172, .F. ) ;
#11117 = ORIENTED_EDGE ( 'NONE', *, *, #17520, .T. ) ;
#11118 = FACE_OUTER_BOUND ( 'NONE', #11516, .T. ) ;
#11119 = EDGE_CURVE ( 'NONE', #15680, #9496, #482, .T. ) ;
#11120=STYLED_ITEM('',(#20988),#17843);
#11121 = CARTESIAN_POINT ( 'NONE',  ( 225.8347918004686221, 42.90510997604505405, -14.99564532486971125 ) ) ;
#11122 = AXIS2_PLACEMENT_3D ( 'NONE', #3938, #18785, #15518 ) ;
#11123 = DIRECTION ( 'NONE',  ( -0.5000000000000047740, 0.8660254037844358210, 0.000000000000000000 ) ) ;
#11124 = CARTESIAN_POINT ( 'NONE',  ( 221.1519434606206005, 33.18250674572787062, -11.35524774226752598 ) ) ;
#11125 = CARTESIAN_POINT ( 'NONE',  ( 220.2746439056042789, 33.18852776005017091, -17.77545290933962363 ) ) ;
#11126 = EDGE_LOOP ( 'NONE', ( #12384, #7260 ) ) ;
#11127 = DIRECTION ( 'NONE',  ( -0.8660254037844360431, -0.5000000000000044409, 5.976026924694052093E-17 ) ) ;
#11128 = CARTESIAN_POINT ( 'NONE',  ( 227.9553588074475954, 39.88513931160571957, -14.00000000000005507 ) ) ;
#11129 = CARTESIAN_POINT ( 'NONE',  ( 32.36389338619004263, 157.9004617752989930, -29.00000000000000000 ) ) ;
#11130 = B_SPLINE_CURVE_WITH_KNOTS ( 'NONE', 3,
 ( #6733, #9610, #13230, #8015 ),
 .UNSPECIFIED., .F., .F.,
 ( 4, 4 ),
 ( 1.393710185265659229E-05, 0.0005798633241500747437 ),
 .UNSPECIFIED. ) ;
#11131 = ORIENTED_EDGE ( 'NONE', *, *, #263, .F. ) ;
#11132 = CARTESIAN_POINT ( 'NONE',  ( 82.93030480524085135, 62.75708420226636264, 0.4611002339714860843 ) ) ;
#11133 = ORIENTED_EDGE ( 'NONE', *, *, #2373, .T. ) ;
#11134 = CIRCLE ( 'NONE', #17909, 5.000000000000001776 ) ;
#11135 = EDGE_LOOP ( 'NONE', ( #4407, #2066, #17167, #17497 ) ) ;
#11136 = CARTESIAN_POINT ( 'NONE',  ( -3.771940362451076556, 64.24999999999997158, 3.997049355788893976 ) ) ;
#11137 = DIRECTION ( 'NONE',  ( -0.8660254037844358210, -0.5000000000000049960, 0.000000000000000000 ) ) ;
#11138 = ORIENTED_EDGE ( 'NONE', *, *, #12783, .F. ) ;
#11139 = APPLICATION_PROTOCOL_DEFINITION ( 'draft international standard', 'automotive_design', 1998, #6880 ) ;
#11140 = CARTESIAN_POINT ( 'NONE',  ( 209.8428577672754898, 12.26951880167198894, -25.15316579317395096 ) ) ;
#11141 = EDGE_LOOP ( 'NONE', ( #11256, #3904, #2947, #17104 ) ) ;
#11142 = PRESENTATION_STYLE_ASSIGNMENT (( #17514 ) ) ;
#11143 = CARTESIAN_POINT ( 'NONE',  ( 202.6226596002730389, 0.8549378841442712984, -23.57241037536569195 ) ) ;
#11144 = CARTESIAN_POINT ( 'NONE',  ( 211.2576524688788311, 27.65102446918777090, -15.10969539796795580 ) ) ;
#11145 = DIRECTION ( 'NONE',  ( -0.5000000000000049960, 0.8660254037844357100, -0.000000000000000000 ) ) ;
#11146 = AXIS2_PLACEMENT_3D ( 'NONE', #19896, #5470, #17910 ) ;
#11147 = DIRECTION ( 'NONE',  ( -1.000000000000000000, -0.000000000000000000, -0.000000000000000000 ) ) ;
#11148 = DIRECTION ( 'NONE',  ( 0.5000000000000049960, -0.8660254037844357100, 0.000000000000000000 ) ) ;
#11149 = CYLINDRICAL_SURFACE ( 'NONE', #17296, 1.499999999999993783 ) ;
#11150 = FACE_OUTER_BOUND ( 'NONE', #18116, .T. ) ;
#11151 = DIRECTION ( 'NONE',  ( -0.8660254037844355990, -0.5000000000000051070, 0.000000000000000000 ) ) ;
#11152 = CARTESIAN_POINT ( 'NONE',  ( 202.6868825351897669, 7.960997897939990686, -25.79243801023027061 ) ) ;
#11153 = ORIENTED_EDGE ( 'NONE', *, *, #2637, .F. ) ;
#11154 = CARTESIAN_POINT ( 'NONE',  ( 205.5965122587965084, 9.994899983462953941, -14.00000000000005507 ) ) ;
#11155 = CARTESIAN_POINT ( 'NONE',  ( 58.69187849547078883, 85.41088488089633302, -11.24813091999954295 ) ) ;
#11156 = EDGE_CURVE ( 'NONE', #6192, #14773, #11926, .T. ) ;
#11157 = CARTESIAN_POINT ( 'NONE',  ( 220.8838919191435650, 34.26463400395766001, -10.33191597617941326 ) ) ;
#11158 = DIRECTION ( 'NONE',  ( -0.000000000000000000, 1.000000000000000000, -0.000000000000000000 ) ) ;
#11159 = AXIS2_PLACEMENT_3D ( 'NONE', #19390, #9933, #13247 ) ;
#11161 = ORIENTED_EDGE ( 'NONE', *, *, #14196, .F. ) ;
#11160 = ORIENTED_EDGE ( 'NONE', *, *, #11984, .F. ) ;
#11162 = ORIENTED_EDGE ( 'NONE', *, *, #1306, .T. ) ;
#11163 = FACE_OUTER_BOUND ( 'NONE', #7523, .T. ) ;
#11164 = AXIS2_PLACEMENT_3D ( 'NONE', #4194, #15353, #807 ) ;
#11165 = AXIS2_PLACEMENT_3D ( 'NONE', #10432, #7357, #16915 ) ;
#11166 = DIRECTION ( 'NONE',  ( -0.5000000000000049960, 0.8660254037844358210, 0.000000000000000000 ) ) ;
#11167 = VERTEX_POINT ( 'NONE', #15124 ) ;
#11168 = DIRECTION ( 'NONE',  ( -0.8660254037844357100, -0.5000000000000051070, 0.000000000000000000 ) ) ;
#11169 = CARTESIAN_POINT ( 'NONE',  ( -26.55686023345718638, 79.99999999967671727, -6.747797645781123066 ) ) ;
#11170 = CARTESIAN_POINT ( 'NONE',  ( 229.7650217427808172, 36.75071116303467988, -13.95414044509044160 ) ) ;
#11171 = AXIS2_PLACEMENT_3D ( 'NONE', #12055, #18519, #20101 ) ;
#11172 = VERTEX_POINT ( 'NONE', #7031 ) ;
#11173 = EDGE_LOOP ( 'NONE', ( #18387, #252 ) ) ;
#11174 = B_SPLINE_CURVE_WITH_KNOTS ( 'NONE', 3,
 ( #1007, #7451, #20395, #5860 ),
 .UNSPECIFIED., .F., .F.,
 ( 4, 4 ),
 ( 0.000000000000000000, 0.001416029653785000168 ),
 .UNSPECIFIED. ) ;
#11175 = DIRECTION ( 'NONE',  ( 0.8660254037844355990, 0.5000000000000054401, 0.000000000000000000 ) ) ;
#11176 = ORIENTED_EDGE ( 'NONE', *, *, #7965, .T. ) ;
#11177 = LINE ( 'NONE', #4706, #10518 ) ;
#11178 = FACE_OUTER_BOUND ( 'NONE', #18616, .T. ) ;
#11179 =( GEOMETRIC_REPRESENTATION_CONTEXT ( 3 ) GLOBAL_UNCERTAINTY_ASSIGNED_CONTEXT ( ( #4499 ) ) GLOBAL_UNIT_ASSIGNED_CONTEXT ( ( #54, #11389, #16375 ) ) REPRESENTATION_CONTEXT ( 'NONE', 'WORKASPACE' ) );
#11180 = CARTESIAN_POINT ( 'NONE',  ( 205.5965122587965084, 9.994899983462953941, -14.00000000000005507 ) ) ;
#11181 = ADVANCED_FACE ( 'NONE', ( #2701 ), #12243, .T. ) ;
#11182 = CARTESIAN_POINT ( 'NONE',  ( 216.3683575532813848, 33.19538101841231992, -14.00000000000004441 ) ) ;
#11183 = AXIS2_PLACEMENT_3D ( 'NONE', #13198, #8294, #9578 ) ;
#11184 = EDGE_CURVE ( 'NONE', #19244, #5690, #1317, .T. ) ;
#11185 = EDGE_LOOP ( 'NONE', ( #19676, #8709, #15565, #12969 ) ) ;
#11186 = DIRECTION ( 'NONE',  ( 0.5000000000000045519, -0.8660254037844360431, 0.000000000000000000 ) ) ;
#11187 = ORIENTED_EDGE ( 'NONE', *, *, #20050, .F. ) ;
#11188 = CARTESIAN_POINT ( 'NONE',  ( 210.1532566776551789, 29.23042781764359432, -11.51600929819806396 ) ) ;
#11189 = CARTESIAN_POINT ( 'NONE',  ( 218.3216332057867248, 38.08474790828346102, -15.46846178913018477 ) ) ;
#11190 = LINE ( 'NONE', #11297, #13778 ) ;
#11191 = CIRCLE ( 'NONE', #1041, 3.902363844300875240 ) ;
#11192 = EDGE_CURVE ( 'NONE', #950, #4518, #2422, .T. ) ;
#11193 = DIRECTION ( 'NONE',  ( 0.8660254037844372643, 0.5000000000000027756, -0.000000000000000000 ) ) ;
#11194 = CARTESIAN_POINT ( 'NONE',  ( -29.99999999999979039, 5.000000000000174971, -2.366409145735037800 ) ) ;
#11195 = VECTOR ( 'NONE', #13878, 1000.000000000000114 ) ;
#11196 = ORIENTED_EDGE ( 'NONE', *, *, #3382, .T. ) ;
#11197 = VECTOR ( 'NONE', #20744, 1000.000000000000000 ) ;
#11198 = CARTESIAN_POINT ( 'NONE',  ( 211.9579643972498673, 13.49067618385247158, -23.74217242726248145 ) ) ;
#11199 = EDGE_CURVE ( 'NONE', #1138, #1467, #16689, .T. ) ;
#11200 = CONICAL_SURFACE ( 'NONE', #6430, 13.07248899748297433, 0.6693469023067423196 ) ;
#11201 = ORIENTED_EDGE ( 'NONE', *, *, #9238, .T. ) ;
#11202 = DIRECTION ( 'NONE',  ( 0.05035489893517486326, 0.02907241445524025303, 0.9983081582712680646 ) ) ;
#11203 = CARTESIAN_POINT ( 'NONE',  ( 0.3663305609645054473, 50.73190751614451699, -7.824425459317669862 ) ) ;
#11204 = PLANE ( 'NONE',  #7220 ) ;
#11205 = AXIS2_PLACEMENT_3D ( 'NONE', #12146, #10215, #8420 ) ;
#11206 = EDGE_CURVE ( 'NONE', #1032, #6628, #13949, .T. ) ;
#11207 = LINE ( 'NONE', #8215, #3708 ) ;
#11208 = AXIS2_PLACEMENT_3D ( 'NONE', #2202, #3570, #13337 ) ;
#11209 = CARTESIAN_POINT ( 'NONE',  ( 205.5965122587965084, 9.994899983462952164, -14.00000000000005507 ) ) ;
#11211 = VERTEX_POINT ( 'NONE', #4284 ) ;
#11210 = VERTEX_POINT ( 'NONE', #9349 ) ;
#11212 = ORIENTED_EDGE ( 'NONE', *, *, #20621, .T. ) ;
#11213 = CARTESIAN_POINT ( 'NONE',  ( 228.3010954329995741, 39.28630591011256001, -10.44704522969155391 ) ) ;
#11214 = CARTESIAN_POINT ( 'NONE',  ( 219.7596605364519746, 36.00588181227283968, -10.27986985910184004 ) ) ;
#11215 = CARTESIAN_POINT ( 'NONE',  ( -0.7874873115017846370, 78.92002130297213114, -6.902655774461555538 ) ) ;
#11216 = VECTOR ( 'NONE', #13303, 1000.000000000000227 ) ;
#11217 = ORIENTED_EDGE ( 'NONE', *, *, #17858, .F. ) ;
#11218 = EDGE_LOOP ( 'NONE', ( #13822, #14372, #16224, #1245 ) ) ;
#11219 = CARTESIAN_POINT ( 'NONE',  ( 48.48114019555096377, 209.9845714233581191, 45.12705109663953351 ) ) ;
#11220 = LINE ( 'NONE', #14735, #8497 ) ;
#11221 = ADVANCED_FACE ( 'NONE', ( #4180 ), #12456, .T. ) ;
#11222 = CARTESIAN_POINT ( 'NONE',  ( 61.99529059433385925, 216.5773763115390125, -22.00000000000000355 ) ) ;
#11223 = DIRECTION ( 'NONE',  ( -0.8660254037844355990, -0.5000000000000055511, 0.000000000000000000 ) ) ;
#11224 = ORIENTED_EDGE ( 'NONE', *, *, #1320, .T. ) ;
#11225 = ADVANCED_FACE ( 'NONE', ( #9244 ), #19350, .T. ) ;
#11226 = ADVANCED_FACE ( 'NONE', ( #20281 ), #5743, .T. ) ;
#11227 = ORIENTED_EDGE ( 'NONE', *, *, #16519, .T. ) ;
#11228 = DIRECTION ( 'NONE',  ( 0.000000000000000000, -1.000000000000000000, 0.000000000000000000 ) ) ;
#11229 =( NAMED_UNIT ( * ) SI_UNIT ( $, .STERADIAN. ) SOLID_ANGLE_UNIT ( ) );
#11230 = AXIS2_PLACEMENT_3D ( 'NONE', #6824, #581, #13409 ) ;
#11231 = VECTOR ( 'NONE', #3710, 1000.000000000000114 ) ;
#11232 = CARTESIAN_POINT ( 'NONE',  ( 218.1772659767879361, 38.33479928385730062, -13.56204498775452372 ) ) ;
#11233 = CIRCLE ( 'NONE', #4791, 11.98469917212512215 ) ;
#11234 = EDGE_CURVE ( 'NONE', #6984, #17847, #18448, .T. ) ;
#11235 = AXIS2_PLACEMENT_3D ( 'NONE', #10371, #853, #20348 ) ;
#11236 = DIRECTION ( 'NONE',  ( 3.965082230804136136E-15, 7.930164461608272272E-15, 1.000000000000000000 ) ) ;
#11237 = CARTESIAN_POINT ( 'NONE',  ( -28.70953045725249453, 62.08313086074902287, 2.221255103732576064 ) ) ;
#11238 = CARTESIAN_POINT ( 'NONE',  ( 69.72421256244413712, 71.31772771003116418, -23.89306908104443394 ) ) ;
#11239 = AXIS2_PLACEMENT_3D ( 'NONE', #7673, #20911, #6385 ) ;
#11240 = ORIENTED_EDGE ( 'NONE', *, *, #2378, .F. ) ;
#11241 = CARTESIAN_POINT ( 'NONE',  ( -27.29745750913661340, 65.65291453363863639, 5.349528374469362468 ) ) ;
#11242 = CARTESIAN_POINT ( 'NONE',  ( 10.49211908931699178, 5.000000000000000000, 0.000000000000000000 ) ) ;
#11243 = CARTESIAN_POINT ( 'NONE',  ( 197.6756539743620351, 9.545788238134468529, -23.47937149798923073 ) ) ;
#11244 = ORIENTED_EDGE ( 'NONE', *, *, #4314, .F. ) ;
#11245 = ADVANCED_FACE ( 'NONE', ( #17215 ), #17427, .T. ) ;
#11246 = CARTESIAN_POINT ( 'NONE',  ( 58.72203124118109940, 85.38772223162817454, -11.09829540933401582 ) ) ;
#11247 = AXIS2_PLACEMENT_3D ( 'NONE', #6372, #1729, #12869 ) ;
#11248 = VERTEX_POINT ( 'NONE', #18595 ) ;
#11249 = VERTEX_POINT ( 'NONE', #4065 ) ;
#11250 = CARTESIAN_POINT ( 'NONE',  ( -3.810871963545228613, 76.46633113979204666, 2.786148689275818935 ) ) ;
#11251 = CARTESIAN_POINT ( 'NONE',  ( 26.99999999999999645, 65.00000000000000000, -22.50000000000000000 ) ) ;
#11252 = CIRCLE ( 'NONE', #2109, 6.960520131757800932 ) ;
#11253 = EDGE_CURVE ( 'NONE', #15055, #2247, #10524, .T. ) ;
#11254 = CARTESIAN_POINT ( 'NONE',  ( 89.99529059433416478, 168.0799536996104848, 21.00000000000000711 ) ) ;
#11255 = FACE_OUTER_BOUND ( 'NONE', #8325, .T. ) ;
#11256 = ORIENTED_EDGE ( 'NONE', *, *, #18704, .T. ) ;
#11257 = LINE ( 'NONE', #943, #18905 ) ;
#11258 = LINE ( 'NONE', #7951, #6049 ) ;
#11259 = DIRECTION ( 'NONE',  ( -0.5000000000000041078, 0.8660254037844363761, 0.000000000000000000 ) ) ;
#11260 = CARTESIAN_POINT ( 'NONE',  ( 199.2144802262915846, 21.04890371929339921, -14.00000000000005507 ) ) ;
#11261 = EDGE_LOOP ( 'NONE', ( #5504, #20615, #1137, #10850 ) ) ;
#11262 = CARTESIAN_POINT ( 'NONE',  ( 82.49529059433407951, 181.0703347563770365, 11.00000000000001066 ) ) ;
#11263 = CARTESIAN_POINT ( 'NONE',  ( 198.6701878702990030, 10.11998265067189529, -3.762296834228767484 ) ) ;
#11264 = CIRCLE ( 'NONE', #17700, 12.00000000000000178 ) ;
#11265 = CARTESIAN_POINT ( 'NONE',  ( 191.5478494775925640, 36.18576207517880050, -14.00000000000006395 ) ) ;
#11266 = CIRCLE ( 'NONE', #18039, 5.000000000000005329 ) ;
#11267 = CARTESIAN_POINT ( 'NONE',  ( 10.40000000000000036, 0.000000000000000000, 0.000000000000000000 ) ) ;
#11268 = DIRECTION ( 'NONE',  ( -0.000000000000000000, -1.000000000000000000, -0.000000000000000000 ) ) ;
#11269 = ORIENTED_EDGE ( 'NONE', *, *, #2524, .F. ) ;
#11270 = DIRECTION ( 'NONE',  ( 0.5000000000000047740, -0.8660254037844359321, 0.000000000000000000 ) ) ;
#11271 = CARTESIAN_POINT ( 'NONE',  ( 82.67991938068482227, 64.19136817925864591, 0.5957706602028168819 ) ) ;
#11272 = CARTESIAN_POINT ( 'NONE',  ( 205.5889925535339557, 2.567551013215509936, -1.381056684022587078 ) ) ;
#11273 = CARTESIAN_POINT ( 'NONE',  ( 219.3925639124447287, 34.71633512454243231, -17.56803216753791475 ) ) ;
#11275 = VERTEX_POINT ( 'NONE', #4877 ) ;
#11274 = ORIENTED_EDGE ( 'NONE', *, *, #15439, .T. ) ;
#11276 = ORIENTED_EDGE ( 'NONE', *, *, #9720, .T. ) ;
#11277 = LINE ( 'NONE', #15954, #18352 ) ;
#11278 = ORIENTED_EDGE ( 'NONE', *, *, #7177, .T. ) ;
#11279 = AXIS2_PLACEMENT_3D ( 'NONE', #8974, #7596, #7377 ) ;
#11280 = PLANE ( 'NONE',  #14801 ) ;
#11281 = EDGE_LOOP ( 'NONE', ( #3520, #2334, #16867, #14202 ) ) ;
#11282 = DIRECTION ( 'NONE',  ( -0.8660254037844355990, -0.5000000000000054401, -1.599177586275613688E-14 ) ) ;
#11283 = ADVANCED_FACE ( 'NONE', ( #12951 ), #10885, .T. ) ;
#11284 = PLANE ( 'NONE',  #11929 ) ;
#11285 = CARTESIAN_POINT ( 'NONE',  ( 228.9326935426791749, 38.19234589418311998, -10.22226263383621614 ) ) ;
#11286 = CARTESIAN_POINT ( 'NONE',  ( 225.9771417706670888, 42.98504265174197059, -14.54471643454050955 ) ) ;
#11287 = ORIENTED_EDGE ( 'NONE', *, *, #17549, .T. ) ;
#11288 = CIRCLE ( 'NONE', #1813, 5.000000000000000888 ) ;
#11289 = LINE ( 'NONE', #4400, #18962 ) ;
#11290 = DIRECTION ( 'NONE',  ( 0.000000000000000000, 1.000000000000000000, 6.009258394948607529E-16 ) ) ;
#11291 = VERTEX_POINT ( 'NONE', #3286 ) ;
#11292 = DIRECTION ( 'NONE',  ( 0.5000000000000057732, -0.8660254037844352659, -4.857225732735059248E-17 ) ) ;
#11293 = ADVANCED_FACE ( 'NONE', ( #10677 ), #6145, .T. ) ;
#11294 = ORIENTED_EDGE ( 'NONE', *, *, #14321, .F. ) ;
#11295 = PLANE ( 'NONE',  #10927 ) ;
#11296 = DIRECTION ( 'NONE',  ( 0.5000000000000051070, -0.8660254037844359321, 0.000000000000000000 ) ) ;
#11297 = CARTESIAN_POINT ( 'NONE',  ( 198.5728404875461024, 20.67845284340592471, -26.45271578590682893 ) ) ;
#11298 = CARTESIAN_POINT ( 'NONE',  ( 205.0662616026534693, 10.91332106064940888, -14.00000000000005507 ) ) ;
#11299 = CARTESIAN_POINT ( 'NONE',  ( -26.09894814240073302, 5.223431272791994040, -7.368069150172500414 ) ) ;
#11300 = VECTOR ( 'NONE', #17406, 1000.000000000000000 ) ;
#11301 = AXIS2_PLACEMENT_3D ( 'NONE', #17836, #28, #19412 ) ;
#11302 = EDGE_CURVE ( 'NONE', #12664, #14889, #17175, .T. ) ;
#11303 = EDGE_LOOP ( 'NONE', ( #20837, #13056, #4833, #18130, #448, #12926 ) ) ;
#11304 = EDGE_CURVE ( 'NONE', #6944, #16821, #20639, .T. ) ;
#11305 = DIRECTION ( 'NONE',  ( -0.8296432542242785368, -0.4789947561577507784, -0.2868032327110803803 ) ) ;
#11306 = VERTEX_POINT ( 'NONE', #4230 ) ;
#11307 = DIRECTION ( 'NONE',  ( -0.5000000000000045519, 0.8660254037844360431, 0.000000000000000000 ) ) ;
#11308 = CARTESIAN_POINT ( 'NONE',  ( -3.810806528046885244, 49.99805885029708463, -12.54965585876388268 ) ) ;
#11309 = DIRECTION ( 'NONE',  ( 1.000000000000000000, 0.000000000000000000, 0.000000000000000000 ) ) ;
#11310 = PLANE ( 'NONE',  #12185 ) ;
#11311 = CARTESIAN_POINT ( 'NONE',  ( 97.27623782526788432, 198.9531532459614880, 12.52486517255494824 ) ) ;
#11312 = B_SPLINE_CURVE_WITH_KNOTS ( 'NONE', 3,
 ( #2237, #20141, #11885, #18348 ),
 .UNSPECIFIED., .F., .F.,
 ( 4, 4 ),
 ( 3.625823136733547116E-05, 0.0008902439693512922492 ),
 .UNSPECIFIED. ) ;
#11314 = VERTEX_POINT ( 'NONE', #1163 ) ;
#11313 = EDGE_LOOP ( 'NONE', ( #10930, #9503, #10173, #737 ) ) ;
#11315 = VERTEX_POINT ( 'NONE', #19171 ) ;
#11316 = CARTESIAN_POINT ( 'NONE',  ( 218.5653220041813540, 10.31703753844722016, -9.858802615641375056 ) ) ;
#11317 = CARTESIAN_POINT ( 'NONE',  ( 208.4761278624580711, 5.007259451653140125, -14.00000000000005507 ) ) ;
#11318 = CARTESIAN_POINT ( 'NONE',  ( -12.40988168468657094, 79.99589872788176592, -12.11680902303699803 ) ) ;
#11319 = ORIENTED_EDGE ( 'NONE', *, *, #14796, .F. ) ;
#11320 = VERTEX_POINT ( 'NONE', #13995 ) ;
#11321 = ORIENTED_EDGE ( 'NONE', *, *, #5853, .T. ) ;
#11322 = CARTESIAN_POINT ( 'NONE',  ( 229.6058754501266890, 37.02636062774789139, -11.31761084191180977 ) ) ;
#11323 = CARTESIAN_POINT ( 'NONE',  ( 215.8450800869675277, 15.91191337786571403, -13.97827067520052147 ) ) ;
#11324 = DIRECTION ( 'NONE',  ( 5.951344303839691563E-17, 3.436010235862028595E-17, 1.000000000000000000 ) ) ;
#11325 = CARTESIAN_POINT ( 'NONE',  ( 198.0882619218635057, -1.762997836098331828, -18.44761907388178912 ) ) ;
#11326 = ORIENTED_EDGE ( 'NONE', *, *, #18057, .F. ) ;
#11327 = ORIENTED_EDGE ( 'NONE', *, *, #16488, .F. ) ;
#11328 = CARTESIAN_POINT ( 'NONE',  ( 196.1030895030431225, 19.25254144767176356, -25.94618751764486575 ) ) ;
#11329 = EDGE_CURVE ( 'NONE', #15290, #7006, #15697, .T. ) ;
#11330 = EDGE_CURVE ( 'NONE', #8514, #8072, #65, .T. ) ;
#11331 = AXIS2_PLACEMENT_3D ( 'NONE', #777, #8394, #14897 ) ;
#11332 = DIRECTION ( 'NONE',  ( 0.5000000000000057732, -0.8660254037844352659, 0.000000000000000000 ) ) ;
#11333 = LINE ( 'NONE', #6745, #10190 ) ;
#11334 = CARTESIAN_POINT ( 'NONE',  ( -28.87969541636898541, 58.77009191570905244, 1.174127190111078134 ) ) ;
#11335 = CARTESIAN_POINT ( 'NONE',  ( 80.00000000000000000, 2.894906536710095477E-17, 4.172000000000029907 ) ) ;
#11336 = DIRECTION ( 'NONE',  ( 0.7235536692358585098, 0.4177439057064706307, -0.5495089780708131144 ) ) ;
#11337 = CARTESIAN_POINT ( 'NONE',  ( 59.39721438298058587, 215.0773763115390125, -5.999999999999973355 ) ) ;
#11338 = ADVANCED_FACE ( 'NONE', ( #6219 ), #19070, .F. ) ;
#11339 = ORIENTED_EDGE ( 'NONE', *, *, #14494, .F. ) ;
#11340 = CARTESIAN_POINT ( 'NONE',  ( 62.17486404044439752, 78.42547049926599811, -11.00043863000396094 ) ) ;
#11341 = ORIENTED_EDGE ( 'NONE', *, *, #162, .T. ) ;
#11342 = DIRECTION ( 'NONE',  ( 0.8660254037844361541, 0.5000000000000044409, -5.976026924694052093E-17 ) ) ;
#11343 = FACE_OUTER_BOUND ( 'NONE', #6474, .T. ) ;
#11344 = EDGE_CURVE ( 'NONE', #9451, #9755, #15587, .T. ) ;
#11345 = DIRECTION ( 'NONE',  ( -0.8660254037844354880, -0.5000000000000055511, 0.000000000000000000 ) ) ;
#11346 = ORIENTED_EDGE ( 'NONE', *, *, #17858, .T. ) ;
#11347 = CARTESIAN_POINT ( 'NONE',  ( 225.7469126937013186, 42.73081429532922471, -15.57898118447794822 ) ) ;
#11348 = CONTEXT_DEPENDENT_SHAPE_REPRESENTATION ( #4329, #10230 ) ;
#11349 = EDGE_CURVE ( 'NONE', #9995, #15623, #18678, .T. ) ;
#11350 = DIRECTION ( 'NONE',  ( 0.000000000000000000, 6.938893903907178303E-18, 1.000000000000000000 ) ) ;
#11351 = EDGE_LOOP ( 'NONE', ( #16004, #12299, #17786, #7021 ) ) ;
#11352 = FACE_OUTER_BOUND ( 'NONE', #15794, .T. ) ;
#11353 = CARTESIAN_POINT ( 'NONE',  ( 209.0403034353200269, 31.46832416448081560, -15.25488430973097209 ) ) ;
#11354 = DIRECTION ( 'NONE',  ( -0.8660254037844360431, -0.5000000000000044409, 0.000000000000000000 ) ) ;
#11355 = CYLINDRICAL_SURFACE ( 'NONE', #1550, 12.47473710546057646 ) ;
#11356 = CARTESIAN_POINT ( 'NONE',  ( 220.7941474011230127, 33.80222769952564477, -17.14987233279968848 ) ) ;
#11357 = CLOSED_SHELL ( 'NONE', ( #12534, #11087, #3022, #2912, #19772, #7314, #5729, #17829, #15025, #5257, #10394, #348, #4102, #17723, #4385, #2908, #18336, #1476, #3016, #6515, #10416, #8978, #17734, #4444, #1373, #3308, #20183, #11479, #14745, #5309, #72, #4094, #18634, #20603, #16136, #17077, #14806, #11631, #19399, #7295, #18109, #17914, #5100, #20024, #8332, #9732, #9597, #20055, #1269, #9477, #4501, #14503, #20688, #15731, #16359, #17431, #3676, #7482, #11371, #13573, #3947, #15758, #3548, #18413, #14769, #20663, #11645, #3577 ) ) ;
#11358 = ADVANCED_FACE ( 'NONE', ( #10785 ), #2750, .F. ) ;
#11359 = DIRECTION ( 'NONE',  ( -0.5171545105027588463, -0.2985792958514009166, -0.8021231927550366292 ) ) ;
#11360 = CARTESIAN_POINT ( 'NONE',  ( 69.76867896048976547, 143.1134727143928842, 41.00000000000001421 ) ) ;
#11361 = CARTESIAN_POINT ( 'NONE',  ( 9.014528480800532151, 248.3427481158983596, 1.000000000000018208 ) ) ;
#11362 = EDGE_CURVE ( 'NONE', #1462, #13637, #4024, .T. ) ;
#11363 = AXIS2_PLACEMENT_3D ( 'NONE', #20652, #73, #2967 ) ;
#11364 = ORIENTED_EDGE ( 'NONE', *, *, #15264, .T. ) ;
#11365 = VECTOR ( 'NONE', #8158, 1000.000000000000000 ) ;
#11366 = ORIENTED_EDGE ( 'NONE', *, *, #5970, .F. ) ;
#11367 = CARTESIAN_POINT ( 'NONE',  ( 221.2362506505824058, 33.44835271264494025, -10.92122735228188546 ) ) ;
#11368 = CARTESIAN_POINT ( 'NONE',  ( 66.17935976187501979, 79.62987128376072121, -3.255002524965970423 ) ) ;
#11369 = CARTESIAN_POINT ( 'NONE',  ( 229.2967989854071220, 37.56169676806560886, -16.83383072344321008 ) ) ;
#11370 = CARTESIAN_POINT ( 'NONE',  ( 78.20613919103151090, 52.54607637467318426, -16.26456764023157930 ) ) ;
#11371 = ADVANCED_FACE ( 'NONE', ( #1263 ), #14101, .F. ) ;
#11373 = ORIENTED_EDGE ( 'NONE', *, *, #15511, .T. ) ;
#11372 = ORIENTED_EDGE ( 'NONE', *, *, #3653, .T. ) ;
#11374 = CIRCLE ( 'NONE', #7972, 5.000000000000000000 ) ;
#11375 = EDGE_LOOP ( 'NONE', ( #9990, #5466, #6914, #18804 ) ) ;
#11376 = DIRECTION ( 'NONE',  ( -0.4439426092011871661, 0.7689311547811460423, -0.4600650377311618078 ) ) ;
#11377 = ORIENTED_EDGE ( 'NONE', *, *, #5380, .T. ) ;
#11378 = CIRCLE ( 'NONE', #9328, 5.000000000000008882 ) ;
#11379 = CARTESIAN_POINT ( 'NONE',  ( 227.6776097244820392, 39.38674894399466808, -10.10863206319042362 ) ) ;
#11380 = CIRCLE ( 'NONE', #1232, 4.057500000000000107 ) ;
#11381 = EDGE_CURVE ( 'NONE', #184, #18641, #12499, .T. ) ;
#11382 = CARTESIAN_POINT ( 'NONE',  ( 200.1750369523376492, -0.5581977105158604235, -20.57673792763505460 ) ) ;
#11383 = ORIENTED_EDGE ( 'NONE', *, *, #11065, .F. ) ;
#11384 = DIRECTION ( 'NONE',  ( 0.000000000000000000, 0.8847993391852065903, -0.4659722409944843102 ) ) ;
#11385 = CARTESIAN_POINT ( 'NONE',  ( 80.73926736692914119, 65.37378763963897654, 0.4957099094033766140 ) ) ;
#11386 = DIRECTION ( 'NONE',  ( -0.8660254037844370423, -0.5000000000000026645, 0.000000000000000000 ) ) ;
#11387 = ORIENTED_EDGE ( 'NONE', *, *, #11612, .F. ) ;
#11388 = CIRCLE ( 'NONE', #5271, 1.001129585171333547 ) ;
#11389 =( NAMED_UNIT ( * ) PLANE_ANGLE_UNIT ( ) SI_UNIT ( $, .RADIAN. ) );
#11390 = DIRECTION ( 'NONE',  ( -3.469446951953639334E-16, 6.009258394948607529E-16, -1.000000000000000000 ) ) ;
#11391 = AXIS2_PLACEMENT_3D ( 'NONE', #2103, #2306, #10232 ) ;
#11392 = ORIENTED_EDGE ( 'NONE', *, *, #9282, .T. ) ;
#11393 = AXIS2_PLACEMENT_3D ( 'NONE', #19000, #14032, #9121 ) ;
#11394 = PLANE ( 'NONE',  #6451 ) ;
#11395 = VERTEX_POINT ( 'NONE', #4438 ) ;
#11396 = CARTESIAN_POINT ( 'NONE',  ( 200.6547414633283211, -0.02364095815690154048, -21.78787861992495323 ) ) ;
#11397 = DIRECTION ( 'NONE',  ( 0.000000000000000000, -1.000000000000000000, 0.000000000000000000 ) ) ;
#11398 = DIRECTION ( 'NONE',  ( 0.5000000000000044409, -0.8660254037844360431, 0.000000000000000000 ) ) ;
#11399 = DIRECTION ( 'NONE',  ( 0.000000000000000000, -1.000000000000000000, 1.295896757998782163E-15 ) ) ;
#11400 = CARTESIAN_POINT ( 'NONE',  ( -28.43128979000083234, 8.662912046624729356, -1.352006923338597177 ) ) ;
#11401 = CARTESIAN_POINT ( 'NONE',  ( 218.4514296286660624, 36.34642752079201955, -17.14987233279964229 ) ) ;
#11402 = ORIENTED_EDGE ( 'NONE', *, *, #4890, .T. ) ;
#11403 = AXIS2_PLACEMENT_3D ( 'NONE', #2177, #19758, #8629 ) ;
#11404 = CARTESIAN_POINT ( 'NONE',  ( 66.00360725464794598, 72.95415083537486112, -22.80269511576363328 ) ) ;
#11405 = CARTESIAN_POINT ( 'NONE',  ( 229.6293339343430091, 36.98572934121634859, -16.00491213559321579 ) ) ;
#11406 = ORIENTED_EDGE ( 'NONE', *, *, #10723, .T. ) ;
#11407 = B_SPLINE_CURVE_WITH_KNOTS ( 'NONE', 3,
 ( #13414, #3968, #19860, #5326 ),
 .UNSPECIFIED., .F., .F.,
 ( 4, 4 ),
 ( 3.702528811464445919E-05, 0.0007096760801717362337 ),
 .UNSPECIFIED. ) ;
#11408 = CARTESIAN_POINT ( 'NONE',  ( 225.7469126937013186, 42.73081429532922471, -15.57898118447794822 ) ) ;
#11409 = CARTESIAN_POINT ( 'NONE',  ( -9.201414108834393701, 49.63991447519583033, -10.51578306933696361 ) ) ;
#11410 = DIRECTION ( 'NONE',  ( 0.000000000000000000, -0.4999999999999987232, 0.8660254037844393737 ) ) ;
#11411 = DIRECTION ( 'NONE',  ( 0.000000000000000000, 0.000000000000000000, -1.000000000000000000 ) ) ;
#11412 = CARTESIAN_POINT ( 'NONE',  ( -18.67450410742786815, 45.53668989701726133, -12.21661053328929469 ) ) ;
#11413 = ORIENTED_EDGE ( 'NONE', *, *, #14357, .T. ) ;
#11414 = VERTEX_POINT ( 'NONE', #1365 ) ;
#11415 = DIRECTION ( 'NONE',  ( -0.5000000000000045519, 0.8660254037844360431, 3.469446951953612710E-16 ) ) ;
#11416 = CARTESIAN_POINT ( 'NONE',  ( 196.3164214246273218, 4.637037042251114904, -19.36714384557513924 ) ) ;
#11417 = ORIENTED_EDGE ( 'NONE', *, *, #15115, .F. ) ;
#11418 = EDGE_LOOP ( 'NONE', ( #18778, #17564, #8253, #17644 ) ) ;
#11419 = AXIS2_PLACEMENT_3D ( 'NONE', #8790, #15593, #15495 ) ;
#11420 = EDGE_CURVE ( 'NONE', #14936, #16059, #7713, .T. ) ;
#11421 = PLANE ( 'NONE',  #14644 ) ;
#11422 = AXIS2_PLACEMENT_3D ( 'NONE', #2029, #14984, #4029 ) ;
#11423 = CARTESIAN_POINT ( 'NONE',  ( 214.2742449478047604, 15.00499128741754262, -7.425127016398544555 ) ) ;
#11424 = LINE ( 'NONE', #17903, #13925 ) ;
#11425 = CARTESIAN_POINT ( 'NONE',  ( -11.68625644715183931, 64.25000000000000000, -2.528164662410438357 ) ) ;
#11426 = ORIENTED_EDGE ( 'NONE', *, *, #5645, .T. ) ;
#11427 = AXIS2_PLACEMENT_3D ( 'NONE', #14429, #11435, #4558 ) ;
#11428 = ORIENTED_EDGE ( 'NONE', *, *, #5679, .T. ) ;
#11429 = DIRECTION ( 'NONE',  ( 0.000000000000000000, 0.000000000000000000, 1.000000000000000000 ) ) ;
#11430 = CARTESIAN_POINT ( 'NONE',  ( 215.6692934924029146, 15.81042294017388805, -11.13964600021398432 ) ) ;
#11431 = B_SPLINE_CURVE_WITH_KNOTS ( 'NONE', 3,
 ( #7933, #3656, #6338, #5339 ),
 .UNSPECIFIED., .F., .F.,
 ( 4, 4 ),
 ( 9.556227015513408202E-07, 0.0006736064147546274401 ),
 .UNSPECIFIED. ) ;
#11432 = EDGE_CURVE ( 'NONE', #4705, #1656, #15982, .T. ) ;
#11433 = VECTOR ( 'NONE', #1733, 1000.000000000000114 ) ;
#11434 = DIRECTION ( 'NONE',  ( -0.8660254037844373753, -0.5000000000000022204, 0.000000000000000000 ) ) ;
#11435 = DIRECTION ( 'NONE',  ( -1.000000000000000000, -0.000000000000000000, -0.000000000000000000 ) ) ;
#11436 = CARTESIAN_POINT ( 'NONE',  ( 64.77682424794421934, 73.48778032978390229, -22.35823834978864610 ) ) ;
#11437 = EDGE_LOOP ( 'NONE', ( #4931, #4404, #1170, #16850, #4287 ) ) ;
#11438 = AXIS2_PLACEMENT_3D ( 'NONE', #15705, #7299, #10588 ) ;
#11439 = CARTESIAN_POINT ( 'NONE',  ( 220.9440545760276962, 32.02907446774799638, -16.68624095904345239 ) ) ;
#11440 = DIRECTION ( 'NONE',  ( -1.000000000000000000, -0.000000000000000000, -0.000000000000000000 ) ) ;
#11441 = ORIENTED_EDGE ( 'NONE', *, *, #6909, .T. ) ;
#11442 = CARTESIAN_POINT ( 'NONE',  ( 55.00515713082256042, 77.67739022016017714, -9.611626274830124217 ) ) ;
#11443 = EDGE_CURVE ( 'NONE', #15566, #17110, #3053, .T. ) ;
#11444 = ORIENTED_EDGE ( 'NONE', *, *, #12005, .F. ) ;
#11445 = EDGE_CURVE ( 'NONE', #3819, #7744, #9855, .T. ) ;
#11446 = CARTESIAN_POINT ( 'NONE',  ( 210.3654177961080052, 6.098041503423209164, -1.717498466822859227 ) ) ;
#11447 = DIRECTION ( 'NONE',  ( 0.000000000000000000, 0.000000000000000000, -1.000000000000000000 ) ) ;
#11448 = VECTOR ( 'NONE', #13387, 1000.000000000000227 ) ;
#11449 = ORIENTED_EDGE ( 'NONE', *, *, #1914, .F. ) ;
#11450 = CARTESIAN_POINT ( 'NONE',  ( 229.5104466180464158, 36.53868908091523338, -14.99564532486981427 ) ) ;
#11451 = VECTOR ( 'NONE', #4460, 1000.000000000000000 ) ;
#11452 =( GEOMETRIC_REPRESENTATION_CONTEXT ( 3 ) GLOBAL_UNCERTAINTY_ASSIGNED_CONTEXT ( ( #13836 ) ) GLOBAL_UNIT_ASSIGNED_CONTEXT ( ( #488, #10209, #19967 ) ) REPRESENTATION_CONTEXT ( 'NONE', 'WORKASPACE' ) );
#11453 = DIRECTION ( 'NONE',  ( 0.000000000000000000, 0.000000000000000000, -1.000000000000000000 ) ) ;
#11454 = EDGE_CURVE ( 'NONE', #20019, #15072, #12301, .T. ) ;
#11455 = ORIENTED_EDGE ( 'NONE', *, *, #8222, .F. ) ;
#11456 = DIRECTION ( 'NONE',  ( -0.8660254037844355990, -0.5000000000000055511, 0.000000000000000000 ) ) ;
#11457 = DIRECTION ( 'NONE',  ( 0.5000000000000007772, -0.8660254037844381525, 0.000000000000000000 ) ) ;
#11458 = DIRECTION ( 'NONE',  ( 0.8660254037844355990, 0.5000000000000054401, 0.000000000000000000 ) ) ;
#11459 = PLANE ( 'NONE',  #15682 ) ;
#11460 = EDGE_CURVE ( 'NONE', #7254, #14795, #11130, .T. ) ;
#11461 = CARTESIAN_POINT ( 'NONE',  ( 226.6211368133091923, 39.11482588413117867, -14.00000000000005507 ) ) ;
#11462 = FACE_OUTER_BOUND ( 'NONE', #98, .T. ) ;
#11463 = LINE ( 'NONE', #6362, #8489 ) ;
#11464 = CONICAL_SURFACE ( 'NONE', #7393, 4.509097725792825528, 0.5235987755983015912 ) ;
#11465 = ORIENTED_EDGE ( 'NONE', *, *, #7456, .F. ) ;
#11466 = FACE_OUTER_BOUND ( 'NONE', #928, .T. ) ;
#11467 = ADVANCED_FACE ( 'NONE', ( #6421 ), #12597, .T. ) ;
#11468 = CARTESIAN_POINT ( 'NONE',  ( 61.33030688981697409, 83.38129477918221255, -6.619636938701232154 ) ) ;
#11469 = CARTESIAN_POINT ( 'NONE',  ( 206.6134256523022259, 3.931827829199530999, -26.28791492288515386 ) ) ;
#11470 = CARTESIAN_POINT ( 'NONE',  ( 79.05205211475293936, 54.16676007582333341, -19.73373562583472562 ) ) ;
#11471 = EDGE_CURVE ( 'NONE', #14019, #3348, #19447, .T. ) ;
#11472 = ORIENTED_EDGE ( 'NONE', *, *, #8051, .F. ) ;
#11473 = EDGE_LOOP ( 'NONE', ( #6635, #2092 ) ) ;
#11474 = ORIENTED_EDGE ( 'NONE', *, *, #7302, .T. ) ;
#11475 = UNCERTAINTY_MEASURE_WITH_UNIT (LENGTH_MEASURE( 1.000000000000000082E-05 ), #1003, 'distance_accuracy_value', 'NONE');
#11476 = B_SPLINE_CURVE_WITH_KNOTS ( 'NONE', 3,
 ( #9613, #1991, #291, #9816 ),
 .UNSPECIFIED., .F., .F.,
 ( 4, 4 ),
 ( 4.589663077585729394E-07, 0.0006731097583523744637 ),
 .UNSPECIFIED. ) ;
#11477 = EDGE_CURVE ( 'NONE', #1523, #2651, #14734, .T. ) ;
#11478 = CARTESIAN_POINT ( 'NONE',  ( -32.70485353615134017, 71.96725945621675180, 0.7929198755315589597 ) ) ;
#11479 = ADVANCED_FACE ( 'NONE', ( #1989 ), #11421, .F. ) ;
#11480 = VECTOR ( 'NONE', #11751, 1000.000000000000114 ) ;
#11481 = ORIENTED_EDGE ( 'NONE', *, *, #467, .F. ) ;
#11482 = LINE ( 'NONE', #20906, #5210 ) ;
#11483 = LINE ( 'NONE', #3123, #19361 ) ;
#11484 = EDGE_CURVE ( 'NONE', #15901, #1882, #18002, .T. ) ;
#11485 = CARTESIAN_POINT ( 'NONE',  ( 54.65284698049440237, 77.82709027839986504, -14.62584647385420311 ) ) ;
#11486 = DIRECTION ( 'NONE',  ( 0.8660254037844355990, 0.5000000000000054401, 0.000000000000000000 ) ) ;
#11487 = EDGE_LOOP ( 'NONE', ( #1888, #5714, #1338, #15158 ) ) ;
#11488 = CARTESIAN_POINT ( 'NONE',  ( 219.0539511230835501, 36.78631126217101155, -10.90641968010458740 ) ) ;
#11489 = CARTESIAN_POINT ( 'NONE',  ( 214.8451803045405484, 14.80357170752643370, -7.132002368301448847 ) ) ;
#11490 = CIRCLE ( 'NONE', #1346, 3.902363844300875240 ) ;
#11491 = ORIENTED_EDGE ( 'NONE', *, *, #15516, .F. ) ;
#11492 = CARTESIAN_POINT ( 'NONE',  ( 220.6963894288021493, 32.45804308600664001, -11.78314368930809763 ) ) ;
#11493 = EDGE_CURVE ( 'NONE', #330, #2960, #11233, .T. ) ;
#11494 = VERTEX_POINT ( 'NONE', #13025 ) ;
#11495 = CARTESIAN_POINT ( 'NONE',  ( 209.6021936215576034, 30.22200596923644511, -11.62851498981274290 ) ) ;
#11496 = FACE_OUTER_BOUND ( 'NONE', #8532, .T. ) ;
#11497 = DIRECTION ( 'NONE',  ( 0.5000000000000051070, -0.8660254037844358210, 0.000000000000000000 ) ) ;
#11498 = AXIS2_PLACEMENT_3D ( 'NONE', #4898, #14682, #3311 ) ;
#11499 = EDGE_CURVE ( 'NONE', #14290, #7333, #16645, .T. ) ;
#11500 = CARTESIAN_POINT ( 'NONE',  ( 229.9064957220379597, 36.50567104301210719, -13.97349461567483608 ) ) ;
#11501 = CARTESIAN_POINT ( 'NONE',  ( 200.8776667170992027, -0.1525342266901607846, -21.66653917424381603 ) ) ;
#11502 = PLANE ( 'NONE',  #5546 ) ;
#11503 = EDGE_LOOP ( 'NONE', ( #13887, #3007, #3978, #19802 ) ) ;
#11504 =( BOUNDED_SURFACE ( )  B_SPLINE_SURFACE ( 3, 2, ( 
 ( #5612, #15093, #16763 ),
 ( #2246, #10602, #863 ),
 ( #18567, #9012, #17087 ),
 ( #18672, #967, #4033 ),
 ( #10486, #13485, #8699 ),
 ( #651, #7106, #4149 ),
 ( #18458, #20355, #19932 ),
 ( #8912, #15408, #7313 ),
 ( #5400, #13594, #7414 ),
 ( #765, #5827, #549 ),
 ( #18248, #3933, #10380 ),
 ( #16663, #2144, #6997 ),
 ( #5928, #7735, #9108 ),
 ( #4663, #18883, #11132 ),
 ( #3080, #12631, #17607 ),
 ( #14338, #7838, #9527 ),
 ( #17186, #19093, #7525 ),
 ( #16029, #12430, #1490 ),
 ( #9313, #9215, #20770 ),
 ( #6240, #2774, #19192 ),
 ( #14018, #7936, #4356 ),
 ( #10926, #7632, #10808 ),
 ( #15818, #10705, #12728 ),
 ( #15609, #20460, #14234 ),
 ( #6140, #14130, #17288 ),
 ( #14439, #6034, #12525 ),
 ( #17397, #4565, #20867 ),
 ( #20665, #11031, #17503 ),
 ( #12324, #1182, #1387 ),
 ( #18779, #1077, #4253 ),
 ( #2668, #15719, #20563 ),
 ( #18986, #4464, #2876 ),
 ( #15918, #2979, #1289 ),
 ( #9422, #14858, #8355 ),
 ( #12836, #17714, #16329 ),
 ( #14655, #8247, #11657 ),
 ( #5068, #17919, #12943 ),
 ( #19395, #19696, #9936 ),
 ( #114, #6547, #13046 ),
 ( #11545, #9833, #3181 ),
 ( #14544, #7, #1908 ),
 ( #10037, #16126, #3377 ),
 ( #308, #6441, #6754 ),
 ( #13252, #5169, #1595 ),
 ( #4871, #11340, #18120 ),
 ( #16218, #19485, #3279 ),
 ( #8141, #1804, #3589 ),
 ( #3491, #17808, #16528 ),
 ( #1694, #9735, #4967 ),
 ( #11442, #14755, #2008 ),
 ( #207, #8455, #14959 ),
 ( #13145, #6650, #6340 ),
 ( #16428, #18019, #19293 ),
 ( #4764, #8034, #11246 ),
 ( #9632, #19587, #5273 ),
 ( #6973, #13565, #5482 ),
 ( #12178, #10140, #6869 ),
 ( #18222, #3685, #2219 ),
 ( #10249, #5374, #11976 ),
 ( #7082, #11763, #18433 ),
 ( #8677, #11866, #7284 ),
 ( #16634, #10355, #3902 ),
 ( #13355, #19800, #2431 ),
 ( #526, #18644, #19909 ),
 ( #16843, #4121, #15176 ),
 ( #18331, #3798, #15071 ),
 ( #628, #10576, #2326 ),
 ( #13460, #8781, #2120 ),
 ( #17062, #8572, #16740 ),
 ( #20021, #15279, #735 ),
 ( #7187, #13672, #20122 ),
 ( #5584, #12076, #10459 ),
 ( #18543, #4010, #16946 ),
 ( #8885, #15386, #838 ),
 ( #13774, #20222, #2538 ),
 ( #5688, #8982, #424 ) ),
 .UNSPECIFIED., .F., .F., .T. ) 
 B_SPLINE_SURFACE_WITH_KNOTS ( ( 4, 2, 2, 2, 2, 2, 2, 2, 2, 2, 2, 2, 2, 2, 2, 2, 2, 2, 2, 2, 2, 2, 2, 2, 2, 2, 2, 2, 2, 2, 2, 2, 2, 2, 2, 2, 2, 4 ),
 ( 3, 3 ),
 ( 0.06885390149614811772, 0.07100558591790274987, 0.07315727033965738202, 0.07530895476141200029, 0.07746063918316663244, 0.07853648139404395545, 0.07961232360492126459, 0.08068816581579857372, 0.08176400802667588286, 0.08283985023755319199, 0.08391569244843051500, 0.08499153465930783802, 0.08606737687018514715, 0.08821906129193977930, 0.09037074571369441145, 0.09467411455720366187, 0.09897748340071291229, 0.1032808522442221766, 0.1075842210877314409, 0.1097359055094860592, 0.1118875899312406913, 0.1140392743529953234, 0.1161909587747499417, 0.1172668009856272509, 0.1183426431965045739, 0.1194184854073818969, 0.1204943276182592060, 0.1215701698291365151, 0.1226460120400138243, 0.1237218542508911334, 0.1247976964617684564, 0.1258735386726457794, 0.1269493808835230886, 0.1291010653052777069, 0.1301769075161550160, 0.1312527497270323251, 0.1334044341487869711, 0.1377078029922962354 ),
 ( 0.000000000000000000, 1.000000000000000000 ),
 .UNSPECIFIED. ) 
 GEOMETRIC_REPRESENTATION_ITEM ( )  RATIONAL_B_SPLINE_SURFACE ( (
 ( 1.000000000000000000, 0.9375990638454466675, 1.000000000000000000),
 ( 1.000000000000000000, 0.9424674560013240887, 1.000000000000000000),
 ( 1.000000000000000000, 0.9472454495395411511, 1.000000000000000000),
 ( 1.000000000000000000, 0.9564605845185850663, 1.000000000000000000),
 ( 1.000000000000000000, 0.9608454732134027454, 1.000000000000000000),
 ( 1.000000000000000000, 0.9689919522595137336, 1.000000000000000000),
 ( 1.000000000000000000, 0.9727657420268004396, 1.000000000000000000),
 ( 1.000000000000000000, 0.9796074070863388661, 1.000000000000000000),
 ( 1.000000000000000000, 0.9826776977508318023, 1.000000000000000000),
 ( 1.000000000000000000, 0.9866441197506812255, 1.000000000000000000),
 ( 1.000000000000000000, 0.9878563112346668840, 1.000000000000000000),
 ( 1.000000000000000000, 0.9900012503172416212, 1.000000000000000000),
 ( 1.000000000000000000, 0.9909393653429625637, 1.000000000000000000),
 ( 1.000000000000000000, 0.9925019860915718084, 1.000000000000000000),
 ( 1.000000000000000000, 0.9931248883185653797, 1.000000000000000000),
 ( 1.000000000000000000, 0.9939517895330679531, 1.000000000000000000),
 ( 1.000000000000000000, 0.9941631134692228144, 1.000000000000000000),
 ( 1.000000000000000000, 0.9941219286420546197, 1.000000000000000000),
 ( 1.000000000000000000, 0.9938724371314660022, 1.000000000000000000),
 ( 1.000000000000000000, 0.9929677657768187782, 1.000000000000000000),
 ( 1.000000000000000000, 0.9923039779988552800, 1.000000000000000000),
 ( 1.000000000000000000, 0.9906518461315473312, 1.000000000000000000),
 ( 1.000000000000000000, 0.9896671415157215490, 1.000000000000000000),
 ( 1.000000000000000000, 0.9874184541695402162, 1.000000000000000000),
 ( 1.000000000000000000, 0.9861538891527321660, 1.000000000000000000),
 ( 1.000000000000000000, 0.9819645303139994397, 1.000000000000000000),
 ( 1.000000000000000000, 0.9786329312631978361, 1.000000000000000000),
 ( 1.000000000000000000, 0.9710304362473276552, 1.000000000000000000),
 ( 1.000000000000000000, 0.9667585549851247517, 1.000000000000000000),
 ( 1.000000000000000000, 0.9525417557630343479, 1.000000000000000000),
 ( 1.000000000000000000, 0.9412001842544890362, 1.000000000000000000),
 ( 1.000000000000000000, 0.9146347518846402735, 1.000000000000000000),
 ( 1.000000000000000000, 0.8994101094843396371, 1.000000000000000000),
 ( 1.000000000000000000, 0.8647450005962233899, 1.000000000000000000),
 ( 1.000000000000000000, 0.8453054357499633076, 1.000000000000000000),
 ( 1.000000000000000000, 0.8016942677996606870, 1.000000000000000000),
 ( 1.000000000000000000, 0.7777397233075318272, 1.000000000000000000),
 ( 1.000000000000000000, 0.7387134092132859875, 1.000000000000000000),
 ( 1.000000000000000000, 0.7251826916704574577, 1.000000000000000000),
 ( 1.000000000000000000, 0.6971304047192319331, 1.000000000000000000),
 ( 1.000000000000000000, 0.6826980669419527858, 1.000000000000000000),
 ( 1.000000000000000000, 0.6534760639743609767, 1.000000000000000000),
 ( 1.000000000000000000, 0.6386527339599178399, 1.000000000000000000),
 ( 1.000000000000000000, 0.6090832796716727504, 1.000000000000000000),
 ( 1.000000000000000000, 0.5943263318904800085, 1.000000000000000000),
 ( 1.000000000000000000, 0.5729533508074381443, 1.000000000000000000),
 ( 1.000000000000000000, 0.5659665513975454809, 1.000000000000000000),
 ( 1.000000000000000000, 0.5526995341054916633, 1.000000000000000000),
 ( 1.000000000000000000, 0.5463867916638659450, 1.000000000000000000),
 ( 1.000000000000000000, 0.5346239116712828698, 1.000000000000000000),
 ( 1.000000000000000000, 0.5291736392160848457, 1.000000000000000000),
 ( 1.000000000000000000, 0.5194015973764528615, 1.000000000000000000),
 ( 1.000000000000000000, 0.5150650454058257610, 1.000000000000000000),
 ( 1.000000000000000000, 0.5079781513294042705, 1.000000000000000000),
 ( 1.000000000000000000, 0.5052035616582067901, 1.000000000000000000),
 ( 1.000000000000000000, 0.5013339263629003062, 1.000000000000000000),
 ( 1.000000000000000000, 0.5002393203327387683, 1.000000000000000000),
 ( 1.000000000000000000, 0.4998309580985344502, 1.000000000000000000),
 ( 1.000000000000000000, 0.5005275148352900105, 1.000000000000000000),
 ( 1.000000000000000000, 0.5037041118084196745, 1.000000000000000000),
 ( 1.000000000000000000, 0.5061579591350763296, 1.000000000000000000),
 ( 1.000000000000000000, 0.5125803135669114718, 1.000000000000000000),
 ( 1.000000000000000000, 0.5165482939438740262, 1.000000000000000000),
 ( 1.000000000000000000, 0.5257728359944916496, 1.000000000000000000),
 ( 1.000000000000000000, 0.5310610287513783945, 1.000000000000000000),
 ( 1.000000000000000000, 0.5482655009316232952, 1.000000000000000000),
 ( 1.000000000000000000, 0.5614273505701570244, 1.000000000000000000),
 ( 1.000000000000000000, 0.5823794962627073524, 1.000000000000000000),
 ( 1.000000000000000000, 0.5895723009191430330, 1.000000000000000000),
 ( 1.000000000000000000, 0.6042245744574831212, 1.000000000000000000),
 ( 1.000000000000000000, 0.6117101498696801976, 1.000000000000000000),
 ( 1.000000000000000000, 0.6341532752532395012, 1.000000000000000000),
 ( 1.000000000000000000, 0.6490967219973816649, 1.000000000000000000),
 ( 1.000000000000000000, 0.6931167578513042216, 1.000000000000000000),
 ( 1.000000000000000000, 0.7213744951071011657, 1.000000000000000000),
 ( 1.000000000000000000, 0.7477234448260038358, 1.000000000000000000) ) ) 
 REPRESENTATION_ITEM ( '' )  SURFACE ( )  );
#11505 = CARTESIAN_POINT ( 'NONE',  ( 72.81261327087452173, 74.40654852583290335, -24.22244567122760728 ) ) ;
#11506 = CARTESIAN_POINT ( 'NONE',  ( 4.000000000000000000, 3.518949890710767026, -4.987329993433320396E-15 ) ) ;
#11507 = VECTOR ( 'NONE', #19453, 1000.000000000000114 ) ;
#11508 = ORIENTED_EDGE ( 'NONE', *, *, #343, .F. ) ;
#11509 = DIRECTION ( 'NONE',  ( -0.5000000000000046629, 0.8660254037844359321, 0.000000000000000000 ) ) ;
#11510 = CARTESIAN_POINT ( 'NONE',  ( -3.102165542891348604, 55.17729803629858054, -1.148087882950909355 ) ) ;
#11511 = DIRECTION ( 'NONE',  ( 0.8660254037844355990, 0.5000000000000054401, 0.000000000000000000 ) ) ;
#11512 = B_SPLINE_CURVE_WITH_KNOTS ( 'NONE', 3,
 ( #15319, #5725, #2582, #18688 ),
 .UNSPECIFIED., .F., .F.,
 ( 4, 4 ),
 ( 2.987124294198783904E-07, 0.0004523519542092777068 ),
 .UNSPECIFIED. ) ;
#11513 = FACE_OUTER_BOUND ( 'NONE', #3561, .T. ) ;
#11514 = DIRECTION ( 'NONE',  ( 0.5000000000000007772, -0.8660254037844381525, 0.000000000000000000 ) ) ;
#11516 = EDGE_LOOP ( 'NONE', ( #18851, #20805 ) ) ;
#11515 = ORIENTED_EDGE ( 'NONE', *, *, #12127, .T. ) ;
#11517 = ORIENTED_EDGE ( 'NONE', *, *, #3280, .F. ) ;
#11518 = ORIENTED_EDGE ( 'NONE', *, *, #10376, .T. ) ;
#11519 = CARTESIAN_POINT ( 'NONE',  ( 227.9411836731248115, 38.93022547339379003, -17.81526153211079588 ) ) ;
#11520 = CARTESIAN_POINT ( 'NONE',  ( 208.8107687779841228, 4.427644383670616079, -14.00000000000005507 ) ) ;
#11521 = EDGE_LOOP ( 'NONE', ( #11579, #5491, #5641, #8599 ) ) ;
#11522 = EDGE_LOOP ( 'NONE', ( #3393, #8595, #15542, #8579 ) ) ;
#11523 = CARTESIAN_POINT ( 'NONE',  ( -29.99999999999999645, 5.000000000000000000, 15.00000000000000000 ) ) ;
#11524 = LINE ( 'NONE', #17693, #20336 ) ;
#11525 = DIRECTION ( 'NONE',  ( 0.5000000000000054401, -0.8660254037844354880, 0.000000000000000000 ) ) ;
#11526 = COLOUR_RGB ( '',0.7921568627450980005, 0.8196078431372548767, 0.9333333333333333481 ) ;
#11527 = DIRECTION ( 'NONE',  ( 0.8660254037844360431, 0.5000000000000045519, 0.000000000000000000 ) ) ;
#11528 = ORIENTED_EDGE ( 'NONE', *, *, #1647, .F. ) ;
#11529 = AXIS2_PLACEMENT_3D ( 'NONE', #20587, #2593, #17318 ) ;
#11530 = ORIENTED_EDGE ( 'NONE', *, *, #3555, .T. ) ;
#11531 = DIRECTION ( 'NONE',  ( -1.000000000000000000, -0.000000000000000000, -0.000000000000000000 ) ) ;
#11532 = CIRCLE ( 'NONE', #16270, 10.26794919243111437 ) ;
#11533 = B_SPLINE_CURVE_WITH_KNOTS ( 'NONE', 3,
 ( #4374, #19008, #987, #16813 ),
 .UNSPECIFIED., .F., .F.,
 ( 4, 4 ),
 ( 5.642010595650565963E-05, 0.0009104058439395384603 ),
 .UNSPECIFIED. ) ;
#11534 = LINE ( 'NONE', #13449, #19590 ) ;
#11535 = CIRCLE ( 'NONE', #11208, 4.999999999999997335 ) ;
#11536 = EDGE_CURVE ( 'NONE', #6684, #14685, #18718, .T. ) ;
#11537 = DIRECTION ( 'NONE',  ( 1.051300182579813185E-16, -6.256999452958517077E-17, 1.000000000000000000 ) ) ;
#11538 = CARTESIAN_POINT ( 'NONE',  ( -27.14901402057759938, 45.52498706128694295, -5.662591622423835069 ) ) ;
#11539 = CARTESIAN_POINT ( 'NONE',  ( 225.8572625086515302, 42.53968280922940437, -16.00491213559311987 ) ) ;
#11540 = VECTOR ( 'NONE', #20745, 1000.000000000000227 ) ;
#11541 = CARTESIAN_POINT ( 'NONE',  ( 208.8107687779841228, 4.427644383670616079, -14.00000000000005507 ) ) ;
#11542 = AXIS2_PLACEMENT_3D ( 'NONE', #7910, #6213, #9186 ) ;
#11543 = CARTESIAN_POINT ( 'NONE',  ( 189.0478494775925355, 40.51588909410097727, -14.00000000000006395 ) ) ;
#11544 = ORIENTED_EDGE ( 'NONE', *, *, #7734, .T. ) ;
#11545 = CARTESIAN_POINT ( 'NONE',  ( 59.64661162979547271, 75.69814633436611473, -5.104845358893310703 ) ) ;
#11546 = CIRCLE ( 'NONE', #1406, 0.004059536337672174817 ) ;
#11547 = VERTEX_POINT ( 'NONE', #11219 ) ;
#11548 = VERTEX_POINT ( 'NONE', #187 ) ;
#11549 = CARTESIAN_POINT ( 'NONE',  ( 198.8360742877594589, -1.073648941537930668, -18.15054426878710103 ) ) ;
#11550 = LINE ( 'NONE', #13255, #8666 ) ;
#11551 = EDGE_CURVE ( 'NONE', #10122, #14068, #1572, .T. ) ;
#11552 = TOROIDAL_SURFACE ( 'NONE', #11911, 17.50000000000000000, 5.000000000000000000 ) ;
#11553 = ORIENTED_EDGE ( 'NONE', *, *, #14961, .T. ) ;
#11554 = CARTESIAN_POINT ( 'NONE',  ( 229.6072825732778142, 36.69745434299156983, -14.96398743228921369 ) ) ;
#11555 = VERTEX_POINT ( 'NONE', #16409 ) ;
#11556 = CONTEXT_DEPENDENT_SHAPE_REPRESENTATION ( #19479, #4346 ) ;
#11557 = CONICAL_SURFACE ( 'NONE', #9170, 13.07248899748297433, 0.6693469023067423196 ) ;
#11558 = VECTOR ( 'NONE', #13310, 1000.000000000000000 ) ;
#11559 = AXIS2_PLACEMENT_3D ( 'NONE', #14805, #13201, #14906 ) ;
#11560 = CARTESIAN_POINT ( 'NONE',  ( -28.39840119452017575, 65.74999999999997158, 3.829763509598343330 ) ) ;
#11561 = ORIENTED_EDGE ( 'NONE', *, *, #8412, .F. ) ;
#11562 = DIRECTION ( 'NONE',  ( 0.8660254037844360431, 0.5000000000000044409, 0.000000000000000000 ) ) ;
#11563 = CARTESIAN_POINT ( 'NONE',  ( 226.8653541683588628, 40.79361683593005949, -10.33191597617938484 ) ) ;
#11564 = EDGE_CURVE ( 'NONE', #950, #16219, #14526, .T. ) ;
#11565 = EDGE_CURVE ( 'NONE', #12038, #14068, #16309, .T. ) ;
#11566 = DIRECTION ( 'NONE',  ( -0.8660254037844357100, -0.5000000000000051070, 0.000000000000000000 ) ) ;
#11567 = DIRECTION ( 'NONE',  ( -0.8660254037844360431, -0.5000000000000045519, -4.336808689942049784E-16 ) ) ;
#11568 = EDGE_LOOP ( 'NONE', ( #20899, #15586, #5253, #14472 ) ) ;
#11569 = LINE ( 'NONE', #16548, #15616 ) ;
#11570 = COLOUR_RGB ( '',0.7921568627450980005, 0.8196078431372548767, 0.9333333333333333481 ) ;
#11571 = CARTESIAN_POINT ( 'NONE',  ( 225.9717758497960745, 42.99433669931995183, -13.53336351278488614 ) ) ;
#11572 = DIRECTION ( 'NONE',  ( 0.000000000000000000, 6.938893903907177533E-18, 1.000000000000000000 ) ) ;
#11573 = ORIENTED_EDGE ( 'NONE', *, *, #4376, .T. ) ;
#11574 = CARTESIAN_POINT ( 'NONE',  ( 200.4103230900084895, 6.823642366611345267, -3.481206571632855074 ) ) ;
#11575 = CARTESIAN_POINT ( 'NONE',  ( 190.9712048706970791, 36.57158503910370939, -9.029101044830413869 ) ) ;
#11576 = B_SPLINE_CURVE_WITH_KNOTS ( 'NONE', 3,
 ( #11912, #2262, #8716, #7122 ),
 .UNSPECIFIED., .F., .F.,
 ( 4, 4 ),
 ( 2.508483997137242450E-05, 0.0008790705779558581102 ),
 .UNSPECIFIED. ) ;
#11577 = CARTESIAN_POINT ( 'NONE',  ( 221.4203618348012128, 32.68756767790141282, -15.97403403822092827 ) ) ;
#11578 = CARTESIAN_POINT ( 'NONE',  ( 77.97393021361884280, 52.10713123856947249, -10.75681189255892534 ) ) ;
#11580 = ORIENTED_EDGE ( 'NONE', *, *, #14163, .T. ) ;
#11579 = ORIENTED_EDGE ( 'NONE', *, *, #5319, .T. ) ;
#11581 = VERTEX_POINT ( 'NONE', #12361 ) ;
#11582 = PRODUCT_DEFINITION ( 'UNKNOWN', '', #18932, #17218 ) ;
#11583 = EDGE_LOOP ( 'NONE', ( #3492, #1045, #6002, #9969 ) ) ;
#11584 = EDGE_LOOP ( 'NONE', ( #524, #6074, #4818, #10579 ) ) ;
#11585 = EDGE_CURVE ( 'NONE', #11248, #7589, #18024, .T. ) ;
#11586 = LINE ( 'NONE', #10387, #12075 ) ;
#11587 = ORIENTED_EDGE ( 'NONE', *, *, #17326, .T. ) ;
#11588 = DIRECTION ( 'NONE',  ( -0.5000000000000049960, 0.8660254037844357100, -0.000000000000000000 ) ) ;
#11589 = CARTESIAN_POINT ( 'NONE',  ( -20.99172629426764658, 79.99999999999126032, -11.47115151921912535 ) ) ;
#11590 = AXIS2_PLACEMENT_3D ( 'NONE', #541, #13479, #5393 ) ;
#11591 = DIRECTION ( 'NONE',  ( 0.000000000000000000, 0.000000000000000000, -1.000000000000000000 ) ) ;
#11592 = CARTESIAN_POINT ( 'NONE',  ( 72.49529059433409373, 198.3908428320658004, 11.00000000000001066 ) ) ;
#11593 = ORIENTED_EDGE ( 'NONE', *, *, #18317, .F. ) ;
#11594 = EDGE_CURVE ( 'NONE', #3757, #3717, #4605, .T. ) ;
#11595 = VECTOR ( 'NONE', #7273, 1000.000000000000114 ) ;
#11596 = CARTESIAN_POINT ( 'NONE',  ( 218.2235991490363745, 38.25454787544715174, -14.91677899116112016 ) ) ;
#11597 = EDGE_CURVE ( 'NONE', #4012, #14531, #2817, .T. ) ;
#11598 = CARTESIAN_POINT ( 'NONE',  ( 61.57468973143931379, 74.87077495648827608, -20.95977551465544764 ) ) ;
#11599 = CARTESIAN_POINT ( 'NONE',  ( 59.39721438298058587, 215.0773763115390125, -5.999999999999973355 ) ) ;
#11600 = ORIENTED_EDGE ( 'NONE', *, *, #13180, .F. ) ;
#11601 = PRESENTATION_STYLE_ASSIGNMENT (( #8618 ) ) ;
#11602 = CARTESIAN_POINT ( 'NONE',  ( 190.7433706042750146, 35.72129598111152404, -9.000000000000062172 ) ) ;
#11603 = ADVANCED_FACE ( 'NONE', ( #20604 ), #8873, .T. ) ;
#11604 = DIRECTION ( 'NONE',  ( -0.8660254037844362651, -0.5000000000000043299, 0.000000000000000000 ) ) ;
#11605 = AXIS2_PLACEMENT_3D ( 'NONE', #9849, #3197, #9650 ) ;
#11606 = AXIS2_PLACEMENT_3D ( 'NONE', #17558, #17451, #2930 ) ;
#11608 = EDGE_LOOP ( 'NONE', ( #20354, #2826, #19493, #8769 ) ) ;
#11607 = ORIENTED_EDGE ( 'NONE', *, *, #16252, .F. ) ;
#11609 = FACE_OUTER_BOUND ( 'NONE', #14281, .T. ) ;
#11610 = CARTESIAN_POINT ( 'NONE',  ( 198.6293134455681013, -1.450621593242038099, -12.64773574313024440 ) ) ;
#11611 = DIRECTION ( 'NONE',  ( -0.5000000000000049960, 0.8660254037844358210, -0.000000000000000000 ) ) ;
#11612 = EDGE_CURVE ( 'NONE', #10626, #19834, #11071, .T. ) ;
#11613 = CARTESIAN_POINT ( 'NONE',  ( 82.88348280418499314, 63.23117012791774982, -25.51603149568004270 ) ) ;
#11614 = CARTESIAN_POINT ( 'NONE',  ( -29.99999999999975842, 5.000000000000111022, -6.406390635520961219 ) ) ;
#11615 = LINE ( 'NONE', #19078, #6680 ) ;
#11616 = DIRECTION ( 'NONE',  ( -0.8645602258681711616, -0.4991540791356389728, 0.05814482891047952767 ) ) ;
#11617 = VERTEX_POINT ( 'NONE', #1326 ) ;
#11618 = EDGE_CURVE ( 'NONE', #8848, #15901, #14058, .T. ) ;
#11619 = CARTESIAN_POINT ( 'NONE',  ( 65.85653452118970108, 79.88098746475269252, -21.59168343458891215 ) ) ;
#11620 = EDGE_CURVE ( 'NONE', #13841, #16063, #4188, .T. ) ;
#11621 = CARTESIAN_POINT ( 'NONE',  ( 227.5312376355471145, 39.64027283883993391, -14.00000000000005507 ) ) ;
#11622 = AXIS2_PLACEMENT_3D ( 'NONE', #14748, #10132, #16625 ) ;
#11623 = ORIENTED_EDGE ( 'NONE', *, *, #20728, .T. ) ;
#11624 = DIRECTION ( 'NONE',  ( 0.9987303135603804449, 0.000000000000000000, -0.05037619254751497799 ) ) ;
#11625 = CARTESIAN_POINT ( 'NONE',  ( -3.512777538380836173, 50.29109887172522519, 0.7760323238818376268 ) ) ;
#11626 = DIRECTION ( 'NONE',  ( 2.003086131649568876E-16, -3.469446951953589044E-16, 1.000000000000000000 ) ) ;
#11627 = EDGE_CURVE ( 'NONE', #570, #14216, #18183, .T. ) ;
#11628 = CARTESIAN_POINT ( 'NONE',  ( -33.48481952675158624, 76.25000000000001421, -2.578432583507804132 ) ) ;
#11629 = DIRECTION ( 'NONE',  ( -5.951344303839690331E-17, -3.436010235862032909E-17, -1.000000000000000000 ) ) ;
#11630 = DIRECTION ( 'NONE',  ( 0.3878556453522061243, -0.6717856837524392999, 0.6310879443260593025 ) ) ;
#11631 = ADVANCED_FACE ( 'NONE', ( #6072 ), #16662, .F. ) ;
#11633 = ORIENTED_EDGE ( 'NONE', *, *, #6679, .T. ) ;
#11632 = EDGE_LOOP ( 'NONE', ( #11838, #11518, #5825, #7857 ) ) ;
#11634 = ORIENTED_EDGE ( 'NONE', *, *, #4373, .T. ) ;
#11635 = CARTESIAN_POINT ( 'NONE',  ( 83.78935635788883474, 148.8289471055651063, 58.21056266367804000 ) ) ;
#11636 = CARTESIAN_POINT ( 'NONE',  ( 205.0662616026534693, 10.91332106064940888, -14.00000000000005507 ) ) ;
#11637 = EDGE_CURVE ( 'NONE', #20059, #5621, #10744, .T. ) ;
#11638 = VERTEX_POINT ( 'NONE', #19033 ) ;
#11639 = CARTESIAN_POINT ( 'NONE',  ( -17.22997025788304271, 58.56006360057318005, -4.849479976237960344 ) ) ;
#11640 = DIRECTION ( 'NONE',  ( 0.8660254037844369313, 0.5000000000000029976, -2.775557561562891351E-16 ) ) ;
#11641 = CARTESIAN_POINT ( 'NONE',  ( -11.86574742045090147, 62.48633020609619848, -2.814775708409676280 ) ) ;
#11642 = CIRCLE ( 'NONE', #2501, 4.999999999999997335 ) ;
#11643 = CIRCLE ( 'NONE', #8229, 3.047499999999999876 ) ;
#11644 = ORIENTED_EDGE ( 'NONE', *, *, #20787, .F. ) ;
#11645 = ADVANCED_FACE ( 'NONE', ( #17121 ), #9052, .T. ) ;
#11646 = ORIENTED_EDGE ( 'NONE', *, *, #9668, .T. ) ;
#11647 = CARTESIAN_POINT ( 'NONE',  ( 199.7687975563032410, 10.75426524862079702, -3.125199447383416818 ) ) ;
#11648 = ORIENTED_EDGE ( 'NONE', *, *, #15272, .F. ) ;
#11649 = CARTESIAN_POINT ( 'NONE',  ( 99.99529059433426426, 150.7594456239217777, 21.00000000000000711 ) ) ;
#11650 = ADVANCED_FACE ( 'NONE', ( #7458 ), #2791, .T. ) ;
#11651 = CARTESIAN_POINT ( 'NONE',  ( 22.32500173739932237, 255.2883321626825932, 8.042028396309266469 ) ) ;
#11652 = CARTESIAN_POINT ( 'NONE',  ( -33.12305221259295251, 56.12619721146663210, -0.3853563272486908997 ) ) ;
#11653 = LINE ( 'NONE', #15063, #20755 ) ;
#11654 = CARTESIAN_POINT ( 'NONE',  ( 205.1848235957376403, 9.226162161231169279, -26.45271578590682893 ) ) ;
#11655 = DIRECTION ( 'NONE',  ( -1.000000000000000000, 0.000000000000000000, 0.000000000000000000 ) ) ;
#11656 = VERTEX_POINT ( 'NONE', #10852 ) ;
#11657 = CARTESIAN_POINT ( 'NONE',  ( 66.96769116650702358, 79.01678623947613289, -2.861952279419488487 ) ) ;
#11658 = EDGE_LOOP ( 'NONE', ( #16065, #1849, #19415, #11769 ) ) ;
#11659 = B_SPLINE_CURVE_WITH_KNOTS ( 'NONE', 3,
 ( #10870, #12583, #13862, #2726, #2831, #12477, #14184, #15674, #11084, #17138, #12689, #17240, #1139, #15567, #10760, #2624, #9066, #9268 ),
 .UNSPECIFIED., .F., .F.,
 ( 4, 2, 2, 2, 2, 2, 2, 2, 4 ),
 ( 0.007901880061100961111, 0.008888972354417348093, 0.009876064647733735075, 0.01086315694105012379, 0.01185024923436651077, 0.01283734152768289775, 0.01382443382099928647, 0.01481152611431567345, 0.01579861840763206043 ),
 .UNSPECIFIED. ) ;
#11660 = CARTESIAN_POINT ( 'NONE',  ( -4.695048959678141287, 66.33121464499512854, 5.333703082175816235 ) ) ;
#11661 = CARTESIAN_POINT ( 'NONE',  ( 208.8577037357181894, 4.346350652224121092, -14.00000000000005507 ) ) ;
#11662 = B_SPLINE_CURVE_WITH_KNOTS ( 'NONE', 3,
 ( #18394, #13632, #3863, #16803 ),
 .UNSPECIFIED., .F., .F.,
 ( 4, 4 ),
 ( 1.122767056911022901E-06, 0.0008551085050338230699 ),
 .UNSPECIFIED. ) ;
#11663 = EDGE_CURVE ( 'NONE', #4355, #10895, #15552, .T. ) ;
#11664 = ORIENTED_EDGE ( 'NONE', *, *, #20760, .F. ) ;
#11665 = DIRECTION ( 'NONE',  ( 0.000000000000000000, 0.000000000000000000, -1.000000000000000000 ) ) ;
#11666 = ORIENTED_EDGE ( 'NONE', *, *, #7473, .F. ) ;
#11667 = CYLINDRICAL_SURFACE ( 'NONE', #8917, 15.00000000000000000 ) ;
#11668 = ORIENTED_EDGE ( 'NONE', *, *, #14383, .F. ) ;
#11669 = FACE_OUTER_BOUND ( 'NONE', #16669, .T. ) ;
#11670 = DIRECTION ( 'NONE',  ( 0.5547001962252220419, 0.000000000000000000, -0.8320502943378484950 ) ) ;
#11671 = CARTESIAN_POINT ( 'NONE',  ( 188.4110494209243711, 14.81154003564305199, -14.01558723443171850 ) ) ;
#11672 = DIRECTION ( 'NONE',  ( -0.4999999999999995004, 0.8660254037844390407, 0.000000000000000000 ) ) ;
#11673 = VERTEX_POINT ( 'NONE', #8947 ) ;
#11674 = LINE ( 'NONE', #18038, #19992 ) ;
#11675 = PLANE ( 'NONE',  #13003 ) ;
#11676 = DIRECTION ( 'NONE',  ( -0.5000000000000041078, 0.8660254037844363761, 0.000000000000000000 ) ) ;
#11677 = EDGE_CURVE ( 'NONE', #5830, #14733, #19202, .T. ) ;
#11678 = EDGE_LOOP ( 'NONE', ( #10638, #16307, #19094, #5583, #12989 ) ) ;
#11679 = DIRECTION ( 'NONE',  ( 0.000000000000000000, 1.000000000000000000, 0.000000000000000000 ) ) ;
#11680 = CARTESIAN_POINT ( 'NONE',  ( 202.8019581880755595, 24.48753073112860079, -12.69065112601704293 ) ) ;
#11681 = ORIENTED_EDGE ( 'NONE', *, *, #3494, .T. ) ;
#11682 = LINE ( 'NONE', #11369, #7419 ) ;
#11683 = CARTESIAN_POINT ( 'NONE',  ( 79.35860935848843667, 49.49491951135498624, -12.08921526900124732 ) ) ;
#11685 = ORIENTED_EDGE ( 'NONE', *, *, #9163, .T. ) ;
#11684 = ORIENTED_EDGE ( 'NONE', *, *, #10833, .F. ) ;
#11686 = EDGE_CURVE ( 'NONE', #4595, #13274, #994, .T. ) ;
#11687 = ORIENTED_EDGE ( 'NONE', *, *, #16037, .T. ) ;
#11688 = ORIENTED_EDGE ( 'NONE', *, *, #824, .T. ) ;
#11689 = LINE ( 'NONE', #11794, #14123 ) ;
#11690 = ORIENTED_EDGE ( 'NONE', *, *, #4997, .T. ) ;
#11691 = CARTESIAN_POINT ( 'NONE',  ( 81.43927332018711240, 61.73960023225036764, -25.08884268687368646 ) ) ;
#11692 = AXIS2_PLACEMENT_3D ( 'NONE', #18420, #5358, #3671 ) ;
#11693 = CARTESIAN_POINT ( 'NONE',  ( -22.75605871197916130, 79.99999999991582911, -10.56315151873249647 ) ) ;
#11694 = DIRECTION ( 'NONE',  ( 0.000000000000000000, 0.4999999999999985012, -0.8660254037844394848 ) ) ;
#11695 = LINE ( 'NONE', #8714, #2196 ) ;
#11696 = ORIENTED_EDGE ( 'NONE', *, *, #14627, .T. ) ;
#11697 = AXIS2_PLACEMENT_3D ( 'NONE', #9326, #9544, #11259 ) ;
#11698 = DIRECTION ( 'NONE',  ( 0.000000000000000000, -1.000000000000000000, 0.000000000000000000 ) ) ;
#11699 = CONICAL_SURFACE ( 'NONE', #13746, 10.85470691220533190, 0.8171114040043576665 ) ;
#11700 = EDGE_CURVE ( 'NONE', #2960, #14504, #12381, .T. ) ;
#11701 = CARTESIAN_POINT ( 'NONE',  ( 54.25045881837945672, 77.99799617759832415, -11.96483503560339301 ) ) ;
#11702 = DIRECTION ( 'NONE',  ( 0.000000000000000000, 0.000000000000000000, -1.000000000000000000 ) ) ;
#11703 = EDGE_LOOP ( 'NONE', ( #18717, #13993, #6325, #18530 ) ) ;
#11704 = CARTESIAN_POINT ( 'NONE',  ( 195.8395605881523522, 4.361721309946301695, -9.913166705713630122 ) ) ;
#11705 = CARTESIAN_POINT ( 'NONE',  ( 35.31538279416582071, 262.7883321626826501, 8.042028396309232718 ) ) ;
#11706 = CARTESIAN_POINT ( 'NONE',  ( 217.5814590494791787, 37.85326076503379511, -12.98880265512657850 ) ) ;
#11707 = CARTESIAN_POINT ( 'NONE',  ( -2.548407363833455452, 77.71408077849609697, -4.406821185032912425 ) ) ;
#11708 = EDGE_CURVE ( 'NONE', #15696, #20836, #19044, .T. ) ;
#11709 = VERTEX_POINT ( 'NONE', #19530 ) ;
#11710 = VECTOR ( 'NONE', #5072, 1000.000000000000227 ) ;
#11711 = ADVANCED_FACE ( 'NONE', ( #1635 ), #5126, .T. ) ;
#11712 = DIRECTION ( 'NONE',  ( 0.5000000000000049960, -0.8660254037844358210, 0.000000000000000000 ) ) ;
#11713 = DIRECTION ( 'NONE',  ( 0.8660254037844370423, 0.5000000000000026645, -0.000000000000000000 ) ) ;
#11714 = AXIS2_PLACEMENT_3D ( 'NONE', #7079, #16426, #20018 ) ;
#11715 = CARTESIAN_POINT ( 'NONE',  ( -30.96704536876718095, 79.01393351695151068, -7.140257836325814012 ) ) ;
#11716 = LINE ( 'NONE', #18279, #20848 ) ;
#11717 = CARTESIAN_POINT ( 'NONE',  ( -28.48198157863886948, 6.472551248386185563, 0.7817513343805246873 ) ) ;
#11718 = LINE ( 'NONE', #4073, #6897 ) ;
#11719 = VERTEX_POINT ( 'NONE', #9675 ) ;
#11720 = ADVANCED_FACE ( 'NONE', ( #12878 ), #1536, .F. ) ;
#11721 = CARTESIAN_POINT ( 'NONE',  ( 81.17986817265170885, 58.60139082422833212, -23.83753921867890924 ) ) ;
#11722 = AXIS2_PLACEMENT_3D ( 'NONE', #18392, #378, #15233 ) ;
#11723 = CARTESIAN_POINT ( 'NONE',  ( 220.7506168395117356, 33.87762484391836892, -10.80501622924635186 ) ) ;
#11724 = EDGE_LOOP ( 'NONE', ( #8648, #5199, #1815, #10007 ) ) ;
#11725 = CIRCLE ( 'NONE', #2600, 5.000000000000036415 ) ;
#11726 = CARTESIAN_POINT ( 'NONE',  ( 27.66668267600675435, 64.25000000000000000, 1.813692929321166547 ) ) ;
#11727 = CARTESIAN_POINT ( 'NONE',  ( -3.504048379385980017, 53.26946170535641301, -3.147386235863720128 ) ) ;
#11728 = CARTESIAN_POINT ( 'NONE',  ( 1.439239224086409141, 76.85170763124995119, -3.302610618814554311 ) ) ;
#11729 = AXIS2_PLACEMENT_3D ( 'NONE', #6621, #13218, #8426 ) ;
#11730 = EDGE_CURVE ( 'NONE', #2773, #2539, #11483, .T. ) ;
#11731 = CYLINDRICAL_SURFACE ( 'NONE', #9164, 7.155882939242642848 ) ;
#11732 = CARTESIAN_POINT ( 'NONE',  ( 32.36389338619004263, 157.9004617752989930, -29.00000000000000000 ) ) ;
#11733 = LINE ( 'NONE', #9906, #12035 ) ;
#11735 = ORIENTED_EDGE ( 'NONE', *, *, #17402, .T. ) ;
#11734 = ORIENTED_EDGE ( 'NONE', *, *, #7428, .T. ) ;
#11736 = VERTEX_POINT ( 'NONE', #8188 ) ;
#11737 = DIRECTION ( 'NONE',  ( -0.8660254037844378194, -0.5000000000000013323, -0.000000000000000000 ) ) ;
#11738 = DIRECTION ( 'NONE',  ( -1.000000000000000000, -0.000000000000000000, -0.000000000000000000 ) ) ;
#11739 = ADVANCED_FACE ( 'NONE', ( #6589 ), #14694, .F. ) ;
#11740 = ORIENTED_EDGE ( 'NONE', *, *, #1095, .F. ) ;
#11741 = ORIENTED_EDGE ( 'NONE', *, *, #17815, .F. ) ;
#11742 =( NAMED_UNIT ( * ) SI_UNIT ( $, .STERADIAN. ) SOLID_ANGLE_UNIT ( ) );
#11743 = DIRECTION ( 'NONE',  ( -0.3886714912512298503, -0.2243995901002338311, -0.8936326403234118310 ) ) ;
#11744 = CARTESIAN_POINT ( 'NONE',  ( 42.39721438298049350, 244.5222400402098231, -18.99999999999997513 ) ) ;
#11745 = ORIENTED_EDGE ( 'NONE', *, *, #11686, .F. ) ;
#11746 = DIRECTION ( 'NONE',  ( -1.129794457510891260E-16, 7.616560175797575475E-17, -1.000000000000000000 ) ) ;
#11747 = CIRCLE ( 'NONE', #6304, 12.47473710546057823 ) ;
#11748 = CARTESIAN_POINT ( 'NONE',  ( 218.8765682739957583, 37.74142054458803131, -16.83383072344315678 ) ) ;
#11749 = EDGE_CURVE ( 'NONE', #6648, #3810, #14483, .T. ) ;
#11750 = EDGE_CURVE ( 'NONE', #12839, #15359, #15617, .T. ) ;
#11751 = DIRECTION ( 'NONE',  ( -0.2483788854153071435, -0.1434016163555487389, -0.9579895123154875680 ) ) ;
#11752 = CARTESIAN_POINT ( 'NONE',  ( -15.99999999999999289, 15.09941697557068530, 15.00000000000000000 ) ) ;
#11753 = CARTESIAN_POINT ( 'NONE',  ( -33.12132922318642869, 51.54497531638352115, -5.859852249581638972 ) ) ;
#11754 = LINE ( 'NONE', #3679, #3146 ) ;
#11755 = ADVANCED_FACE ( 'NONE', ( #3424 ), #8287, .T. ) ;
#11756 = DIRECTION ( 'NONE',  ( 0.000000000000000000, 0.000000000000000000, 1.000000000000000000 ) ) ;
#11757 = DIRECTION ( 'NONE',  ( 0.5000000000000046629, -0.8660254037844360431, 0.000000000000000000 ) ) ;
#11758 = AXIS2_PLACEMENT_3D ( 'NONE', #12716, #20648, #9618 ) ;
#11759 = CIRCLE ( 'NONE', #10506, 7.155882939242646401 ) ;
#11761 = VERTEX_POINT ( 'NONE', #17860 ) ;
#11760 = VERTEX_POINT ( 'NONE', #4811 ) ;
#11762 = ORIENTED_EDGE ( 'NONE', *, *, #962, .F. ) ;
#11763 = CARTESIAN_POINT ( 'NONE',  ( 62.83629031002387677, 78.04075569348968600, -12.39075692183127941 ) ) ;
#11764 = ORIENTED_EDGE ( 'NONE', *, *, #8076, .F. ) ;
#11765 = ORIENTED_EDGE ( 'NONE', *, *, #3270, .T. ) ;
#11766 = CARTESIAN_POINT ( 'NONE',  ( 221.2055468244791427, 33.05963819000760395, -11.49787972461438734 ) ) ;
#11767 = LINE ( 'NONE', #19700, #5259 ) ;
#11768 = ADVANCED_FACE ( 'NONE', ( #1845 ), #11284, .F. ) ;
#11769 = ORIENTED_EDGE ( 'NONE', *, *, #2121, .F. ) ;
#11770 = FACE_OUTER_BOUND ( 'NONE', #2122, .T. ) ;
#11771 = CARTESIAN_POINT ( 'NONE',  ( 77.00490953756757051, 160.5799536996104564, 56.00000000000000711 ) ) ;
#11772 = ORIENTED_EDGE ( 'NONE', *, *, #2403, .T. ) ;
#11773 = CIRCLE ( 'NONE', #5669, 13.99999999999998757 ) ;
#11774 = CARTESIAN_POINT ( 'NONE',  ( 137.6791466197848592, 79.48909236273166812, 1.792808077408215874E-16 ) ) ;
#11775 = CARTESIAN_POINT ( 'NONE',  ( 208.1960812450810465, 4.072754371081482638, -2.187257959407754804 ) ) ;
#11776 = CIRCLE ( 'NONE', #11427, 6.500000000000000888 ) ;
#11777 = ORIENTED_EDGE ( 'NONE', *, *, #19257, .T. ) ;
#11778 = CARTESIAN_POINT ( 'NONE',  ( -15.99999999999999289, 9.999999999999994671, 0.000000000000000000 ) ) ;
#11779 = DIRECTION ( 'NONE',  ( -0.000000000000000000, -1.000000000000000000, -0.000000000000000000 ) ) ;
#11780 = ORIENTED_EDGE ( 'NONE', *, *, #12130, .F. ) ;
#11781 = DIRECTION ( 'NONE',  ( 0.000000000000000000, -0.5000000000000022204, -0.8660254037844372643 ) ) ;
#11782 = DIRECTION ( 'NONE',  ( 0.000000000000000000, 0.5000000000000009992, 0.8660254037844380415 ) ) ;
#11783 = DIRECTION ( 'NONE',  ( -0.000000000000000000, 1.000000000000000000, -0.000000000000000000 ) ) ;
#11784 = ORIENTED_EDGE ( 'NONE', *, *, #19219, .F. ) ;
#11785 = CARTESIAN_POINT ( 'NONE',  ( 221.3540177668497222, 33.45035214977922777, -10.82724490084735791 ) ) ;
#11786 = CARTESIAN_POINT ( 'NONE',  ( 199.0852767235472527, -1.187371071960172664, -9.928836400542227381 ) ) ;
#11787 = AXIS2_PLACEMENT_3D ( 'NONE', #6904, #19838, #560 ) ;
#11788 = CARTESIAN_POINT ( 'NONE',  ( -11.79233082830550217, 67.16614382405823847, -2.712160011935105697 ) ) ;
#11789 = CARTESIAN_POINT ( 'NONE',  ( 78.17606435269406973, 52.48910905489428558, -8.931864344943981848 ) ) ;
#11790 = CIRCLE ( 'NONE', #13476, 4.057500000000029416 ) ;
#11792 = ORIENTED_EDGE ( 'NONE', *, *, #14511, .F. ) ;
#11791 = ORIENTED_EDGE ( 'NONE', *, *, #7937, .T. ) ;
#11793 = ORIENTED_EDGE ( 'NONE', *, *, #3004, .F. ) ;
#11794 = CARTESIAN_POINT ( 'NONE',  ( 157.3972143829815309, 45.33639716978957068, -22.00000000000007816 ) ) ;
#11795 = VERTEX_POINT ( 'NONE', #9774 ) ;
#11796 = CARTESIAN_POINT ( 'NONE',  ( 75.32572401052811983, 52.39125122145336633, -9.316704993171171623 ) ) ;
#11797 = CARTESIAN_POINT ( 'NONE',  ( -22.93365594915012906, 79.93797039651411751, -11.02074839552765440 ) ) ;
#11798 = CARTESIAN_POINT ( 'NONE',  ( 4.000000000000000000, 5.278424836066145431, -3.047500000000006093 ) ) ;
#11799 = CARTESIAN_POINT ( 'NONE',  ( 210.7763206480203166, 12.98546375133203767, -24.38552490958320718 ) ) ;
#11800 = ORIENTED_EDGE ( 'NONE', *, *, #16516, .F. ) ;
#11801 = AXIS2_PLACEMENT_3D ( 'NONE', #8923, #7324, #20261 ) ;
#11802 = CARTESIAN_POINT ( 'NONE',  ( 219.1264567230215050, 10.64100881942120580, -12.59769448420680504 ) ) ;
#11803 = FACE_OUTER_BOUND ( 'NONE', #12053, .T. ) ;
#11804 = EDGE_CURVE ( 'NONE', #2174, #4567, #4909, .T. ) ;
#11805 = DIRECTION ( 'NONE',  ( -0.8660254037844370423, -0.5000000000000026645, 0.000000000000000000 ) ) ;
#11806 = EDGE_LOOP ( 'NONE', ( #19021, #18762, #20181, #953 ) ) ;
#11807 = PLANE ( 'NONE',  #5067 ) ;
#11808 = CARTESIAN_POINT ( 'NONE',  ( 195.9478142713745399, 8.548219520498097523, -21.59012016402711254 ) ) ;
#11809 = CARTESIAN_POINT ( 'NONE',  ( 0.3999999999999975797, 0.000000000000000000, 6.099999999999999645 ) ) ;
#11810 = CARTESIAN_POINT ( 'NONE',  ( -10.36721944571354292, 79.98685641808548041, -11.85964839586857700 ) ) ;
#11812 = VERTEX_POINT ( 'NONE', #7880 ) ;
#11811 = ORIENTED_EDGE ( 'NONE', *, *, #2403, .F. ) ;
#11813 = AXIS2_PLACEMENT_3D ( 'NONE', #17491, #16018, #2966 ) ;
#11814 = DIRECTION ( 'NONE',  ( 0.000000000000000000, 0.000000000000000000, -1.000000000000000000 ) ) ;
#11815 = CARTESIAN_POINT ( 'NONE',  ( 34.99529059433359635, 263.3427481158985870, -5.999999999999973355 ) ) ;
#11816 = DIRECTION ( 'NONE',  ( 0.4999999999999995004, -0.8660254037844390407, 0.000000000000000000 ) ) ;
#11817 = PRODUCT_DEFINITION_FORMATION_WITH_SPECIFIED_SOURCE ( 'ANY', '', #17206, .NOT_KNOWN. ) ;
#11818 = LINE ( 'NONE', #16585, #12740 ) ;
#11819 = CARTESIAN_POINT ( 'NONE',  ( -27.12336767588134379, 6.223326257262052685, 5.765760347548625653 ) ) ;
#11820 = PLANE ( 'NONE',  #16404 ) ;
#11821 = VERTEX_POINT ( 'NONE', #6693 ) ;
#11822 = ORIENTED_EDGE ( 'NONE', *, *, #2039, .T. ) ;
#11823 = CARTESIAN_POINT ( 'NONE',  ( 82.60978052030384333, 59.60460182822771458, -24.77599324758051580 ) ) ;
#11824 = DIRECTION ( 'NONE',  ( -0.8660254037844370423, -0.5000000000000026645, 0.000000000000000000 ) ) ;
#11825 = EDGE_CURVE ( 'NONE', #9665, #9995, #20725, .T. ) ;
#11826 = CIRCLE ( 'NONE', #9781, 1.003313105759049417 ) ;
#11827 = VERTEX_POINT ( 'NONE', #5110 ) ;
#11828 = EDGE_CURVE ( 'NONE', #6449, #310, #16167, .T. ) ;
#11829 = CARTESIAN_POINT ( 'NONE',  ( 202.0445642045415582, 25.79900422344375599, -15.30999104003096889 ) ) ;
#11830 = CARTESIAN_POINT ( 'NONE',  ( 0.2566486213402327521, 60.25789211473291118, 1.735236065182640397 ) ) ;
#11831 = CARTESIAN_POINT ( 'NONE',  ( -15.99999999999999289, 80.00000000000000000, -12.50000000000000000 ) ) ;
#11832 = DIRECTION ( 'NONE',  ( 0.8660254037844361541, 0.5000000000000044409, 0.000000000000000000 ) ) ;
#11833 = FACE_OUTER_BOUND ( 'NONE', #18232, .T. ) ;
#11834 = DIRECTION ( 'NONE',  ( -0.8660254037844355990, -0.5000000000000055511, 0.000000000000000000 ) ) ;
#11836 = ORIENTED_EDGE ( 'NONE', *, *, #1889, .F. ) ;
#11835 = ORIENTED_EDGE ( 'NONE', *, *, #16857, .T. ) ;
#11837 = ORIENTED_EDGE ( 'NONE', *, *, #8233, .F. ) ;
#11838 = ORIENTED_EDGE ( 'NONE', *, *, #17793, .T. ) ;
#11839 = LINE ( 'NONE', #8957, #1050 ) ;
#11840 = DIRECTION ( 'NONE',  ( 0.5000000000000007772, -0.8660254037844381525, 0.000000000000000000 ) ) ;
#11841 = ORIENTED_EDGE ( 'NONE', *, *, #15924, .F. ) ;
#11842 = ORIENTED_EDGE ( 'NONE', *, *, #3142, .F. ) ;
#11843 = ADVANCED_FACE ( 'NONE', ( #14585 ), #17542, .F. ) ;
#11844 = CARTESIAN_POINT ( 'NONE',  ( 81.54430079493101857, 62.01789667144628027, 0.1610543161642296051 ) ) ;
#11845 = DIRECTION ( 'NONE',  ( 0.000000000000000000, 6.938893903907177533E-18, 1.000000000000000000 ) ) ;
#11846 = DIRECTION ( 'NONE',  ( -0.8660254037844355990, -0.5000000000000054401, -2.934143223514386573E-14 ) ) ;
#11847 = AXIS2_PLACEMENT_3D ( 'NONE', #8244, #11336, #19481 ) ;
#11848 = ORIENTED_EDGE ( 'NONE', *, *, #1129, .T. ) ;
#11849 = LINE ( 'NONE', #16617, #194 ) ;
#11850 = DIRECTION ( 'NONE',  ( 0.7951984747223580507, 0.4591080534401394408, -0.3960797660391671138 ) ) ;
#11851 = VECTOR ( 'NONE', #9261, 1000.000000000000227 ) ;
#11852 = ADVANCED_FACE ( 'NONE', ( #20808 ), #15668, .T. ) ;
#11853 = AXIS2_PLACEMENT_3D ( 'NONE', #10325, #20094, #20196 ) ;
#11854 = CARTESIAN_POINT ( 'NONE',  ( 218.7874248973968179, 10.18766947982593862, -16.70797078425240301 ) ) ;
#11855 = CIRCLE ( 'NONE', #20318, 11.94520687646042667 ) ;
#11856 = ADVANCED_FACE ( 'NONE', ( #19237 ), #13295, .F. ) ;
#11857 = DIRECTION ( 'NONE',  ( 0.000000000000000000, 0.000000000000000000, -1.000000000000000000 ) ) ;
#11858 = CARTESIAN_POINT ( 'NONE',  ( -26.63192765507035276, 50.95949204697693347, -6.673528889801894515 ) ) ;
#11859 = CARTESIAN_POINT ( 'NONE',  ( 0.000000000000000000, -3.518949890710766581, 4.553649124439118623E-15 ) ) ;
#11860 = EDGE_CURVE ( 'NONE', #10920, #4917, #413, .T. ) ;
#11861 = CARTESIAN_POINT ( 'NONE',  ( 218.1626406098745008, 38.35320191943676349, -14.00000000000005507 ) ) ;
#11862 = FACE_OUTER_BOUND ( 'NONE', #15817, .T. ) ;
#11864 = VERTEX_POINT ( 'NONE', #10188 ) ;
#11863 = ORIENTED_EDGE ( 'NONE', *, *, #3089, .F. ) ;
#11865 = CIRCLE ( 'NONE', #2731, 11.98469917212512215 ) ;
#11866 = CARTESIAN_POINT ( 'NONE',  ( 62.79164080153381633, 78.06686219698755735, -12.37752595184878679 ) ) ;
#11867 = CIRCLE ( 'NONE', #8457, 12.50000000000000000 ) ;
#11868 = ORIENTED_EDGE ( 'NONE', *, *, #11344, .F. ) ;
#11869 = EDGE_CURVE ( 'NONE', #14773, #15680, #17349, .T. ) ;
#11870 = ORIENTED_EDGE ( 'NONE', *, *, #9784, .T. ) ;
#11871 = FACE_BOUND ( 'NONE', #2062, .T. ) ;
#11872 = DIRECTION ( 'NONE',  ( -0.8660254037844354880, -0.5000000000000055511, 0.000000000000000000 ) ) ;
#11873 = AXIS2_PLACEMENT_3D ( 'NONE', #7316, #3828, #5715 ) ;
#11874 = ORIENTED_EDGE ( 'NONE', *, *, #2292, .T. ) ;
#11875 = CARTESIAN_POINT ( 'NONE',  ( 215.6983787324637376, 15.82721531135244675, -16.75125533358882279 ) ) ;
#11876 = AXIS2_PLACEMENT_3D ( 'NONE', #15477, #16735, #5794 ) ;
#11877 = EDGE_CURVE ( 'NONE', #20090, #3073, #1770, .T. ) ;
#11878 = DIRECTION ( 'NONE',  ( 1.000000000000000000, 0.000000000000000000, 0.000000000000000000 ) ) ;
#11879 = ORIENTED_EDGE ( 'NONE', *, *, #17168, .F. ) ;
#11880 = VECTOR ( 'NONE', #7605, 1000.000000000000114 ) ;
#11881 = CARTESIAN_POINT ( 'NONE',  ( 218.1639642825640522, 38.35783849407987844, -13.95097276009430587 ) ) ;
#11882 = DIRECTION ( 'NONE',  ( -1.000000000000000000, -0.000000000000000000, -0.000000000000000000 ) ) ;
#11883 = AXIS2_PLACEMENT_3D ( 'NONE', #15836, #15742, #5951 ) ;
#11884 = DIRECTION ( 'NONE',  ( -0.1674398060854952741, 0.2900142513495578278, 0.9422609221188190665 ) ) ;
#11885 = CARTESIAN_POINT ( 'NONE',  ( 214.9440738535968762, 8.483915958974842297, -23.86786078788951571 ) ) ;
#11886 = DIRECTION ( 'NONE',  ( 0.3654179821390644567, -0.6329225110641519825, -0.6825531432186529024 ) ) ;
#11887 = ADVANCED_FACE ( 'NONE', ( #667 ), #18164, .F. ) ;
#11888 = CIRCLE ( 'NONE', #10860, 8.000000000000000000 ) ;
#11889 = CARTESIAN_POINT ( 'NONE',  ( 10.40000000000000036, 6.613092715395708453E-16, 5.400000000000001243 ) ) ;
#11890 = CARTESIAN_POINT ( 'NONE',  ( 218.9556298744170135, 35.47312707796260867, -10.49174204642374519 ) ) ;
#11891 = CARTESIAN_POINT ( 'NONE',  ( 221.3517569193846271, 32.83641968311255965, -11.78314368930809231 ) ) ;
#11892 = ORIENTED_EDGE ( 'NONE', *, *, #4504, .T. ) ;
#11893 = CARTESIAN_POINT ( 'NONE',  ( 0.000000000000000000, 0.000000000000000000, 6.500000000000000888 ) ) ;
#11894 = AXIS2_PLACEMENT_3D ( 'NONE', #499, #597, #10109 ) ;
#11895 = EDGE_CURVE ( 'NONE', #7807, #15357, #6000, .T. ) ;
#11896 = VECTOR ( 'NONE', #19465, 1000.000000000000000 ) ;
#11897 = PRODUCT_DEFINITION ( 'UNKNOWN', '', #13858, #9565 ) ;
#11898 = DIRECTION ( 'NONE',  ( 0.8660254037844361541, 0.5000000000000044409, -5.976026924694052093E-17 ) ) ;
#11899 = DIRECTION ( 'NONE',  ( 0.000000000000000000, -1.000000000000000000, 0.000000000000000000 ) ) ;
#11901 = ORIENTED_EDGE ( 'NONE', *, *, #1850, .T. ) ;
#11900 = ORIENTED_EDGE ( 'NONE', *, *, #13396, .F. ) ;
#11902 = AXIS2_PLACEMENT_3D ( 'NONE', #12157, #7362, #18618 ) ;
#11903 = AXIS2_PLACEMENT_3D ( 'NONE', #17339, #9258, #1225 ) ;
#11904 = DIRECTION ( 'NONE',  ( -0.7499999999999953371, -0.4330127018922227400, 0.5000000000000039968 ) ) ;
#11905 = ORIENTED_EDGE ( 'NONE', *, *, #18844, .T. ) ;
#11906 = CYLINDRICAL_SURFACE ( 'NONE', #19560, 5.000000000000002665 ) ;
#11907 = CARTESIAN_POINT ( 'NONE',  ( -18.07003674992471431, 79.99999999999891998, -12.33825502280018860 ) ) ;
#11908 = DIRECTION ( 'NONE',  ( -0.8660254037844378194, -0.5000000000000013323, -0.000000000000000000 ) ) ;
#11909 = CARTESIAN_POINT ( 'NONE',  ( 198.4821375217713353, 5.887413813925527428, -22.72623880687287468 ) ) ;
#11910 = ORIENTED_EDGE ( 'NONE', *, *, #1616, .F. ) ;
#11911 = AXIS2_PLACEMENT_3D ( 'NONE', #12790, #11397, #15868 ) ;
#11912 = CARTESIAN_POINT ( 'NONE',  ( 208.2224579217690632, 4.087982952467670295, -25.92587471718749725 ) ) ;
#11913 = AXIS2_PLACEMENT_3D ( 'NONE', #1054, #17265, #4334 ) ;
#11914 = VECTOR ( 'NONE', #19923, 1000.000000000000114 ) ;
#11915 = CARTESIAN_POINT ( 'NONE',  ( 226.1888283990221566, 42.94485973211424579, -14.53509620734043395 ) ) ;
#11916 = CARTESIAN_POINT ( 'NONE',  ( 7.999999999999998224, 5.388445916248354013E-16, 4.400000000000000355 ) ) ;
#11917 = VERTEX_POINT ( 'NONE', #16782 ) ;
#11918 = AXIS2_PLACEMENT_3D ( 'NONE', #3629, #19634, #18063 ) ;
#11919 = DIRECTION ( 'NONE',  ( 0.000000000000000000, 0.9123518090004800740, 0.4094071037653735923 ) ) ;
#11920 = LINE ( 'NONE', #17002, #9818 ) ;
#11921 = CARTESIAN_POINT ( 'NONE',  ( 220.2180084519553134, 35.41797800104779270, -14.00000000000005507 ) ) ;
#11922 = CARTESIAN_POINT ( 'NONE',  ( -2.776596111954927171, 78.20541348178335284, -5.222231676844829806 ) ) ;
#11923=STYLED_ITEM('',(#20974),#3331);
#11924 = ORIENTED_EDGE ( 'NONE', *, *, #9277, .T. ) ;
#11925 = ORIENTED_EDGE ( 'NONE', *, *, #4152, .F. ) ;
#11926 = LINE ( 'NONE', #8627, #4114 ) ;
#11927 = CARTESIAN_POINT ( 'NONE',  ( 93.04593889385130012, 210.2557651598135351, 11.00000000000000888 ) ) ;
#11928 = CYLINDRICAL_SURFACE ( 'NONE', #1592, 12.47473710546057646 ) ;
#11929 = AXIS2_PLACEMENT_3D ( 'NONE', #249, #17753, #3017 ) ;
#11930 = AXIS2_PLACEMENT_3D ( 'NONE', #3370, #11537, #5161 ) ;
#11931 = CARTESIAN_POINT ( 'NONE',  ( 218.4113082942438666, 37.92942609890246786, -15.81459191843834944 ) ) ;
#11932 = EDGE_CURVE ( 'NONE', #16360, #13235, #8509, .T. ) ;
#11933 = CARTESIAN_POINT ( 'NONE',  ( -26.20390737937308501, 9.999999997134366936, 7.228123494169216734 ) ) ;
#11934 =( NAMED_UNIT ( * ) PLANE_ANGLE_UNIT ( ) SI_UNIT ( $, .RADIAN. ) );
#11935 = LINE ( 'NONE', #5649, #3878 ) ;
#11936 = VERTEX_POINT ( 'NONE', #2364 ) ;
#11937 = CARTESIAN_POINT ( 'NONE',  ( 80.80276550169267580, 60.34984310387103790, -24.64969702106051841 ) ) ;
#11938 = CYLINDRICAL_SURFACE ( 'NONE', #2571, 1.499999999999990896 ) ;
#11939 = VERTEX_POINT ( 'NONE', #18264 ) ;
#11940 = CARTESIAN_POINT ( 'NONE',  ( 201.8620183822125398, 26.37541784318060678, -14.66741346640867150 ) ) ;
#11941 = CARTESIAN_POINT ( 'NONE',  ( -3.331652052620986737, 63.24197008610744319, 2.417743185958345364 ) ) ;
#11942 = CARTESIAN_POINT ( 'NONE',  ( 218.4231237361075841, 38.52680952262490166, -12.46964089162983313 ) ) ;
#11943 = VECTOR ( 'NONE', #19714, 1000.000000000000114 ) ;
#11944 = DIRECTION ( 'NONE',  ( -0.5000000000000005551, 0.8660254037844382635, 0.000000000000000000 ) ) ;
#11945 = CARTESIAN_POINT ( 'NONE',  ( 96.88087538439039292, 198.6134603144004132, 10.83638872456144675 ) ) ;
#11946 = EDGE_CURVE ( 'NONE', #20315, #1201, #17680, .T. ) ;
#11947 = CIRCLE ( 'NONE', #19013, 3.845804376225747667 ) ;
#11948 = CYLINDRICAL_SURFACE ( 'NONE', #9684, 6.500000000000000000 ) ;
#11950 = ORIENTED_EDGE ( 'NONE', *, *, #10282, .T. ) ;
#11949 = ORIENTED_EDGE ( 'NONE', *, *, #14163, .F. ) ;
#11951 = ORIENTED_EDGE ( 'NONE', *, *, #5381, .F. ) ;
#11952 = DIRECTION ( 'NONE',  ( 1.000000000000000000, 0.000000000000000000, 0.000000000000000000 ) ) ;
#11953 = DIRECTION ( 'NONE',  ( 0.6634139481689433904, 0.3830222215594970003, 0.6427876096865293709 ) ) ;
#11954 = ORIENTED_EDGE ( 'NONE', *, *, #9087, .F. ) ;
#11955 = CARTESIAN_POINT ( 'NONE',  ( 5.000000000000000000, 2.342598717236900718, -4.057500000000001883 ) ) ;
#11956 = CARTESIAN_POINT ( 'NONE',  ( 69.50490953756755630, 173.5703347563769796, 16.00000000000001066 ) ) ;
#11957 = CARTESIAN_POINT ( 'NONE',  ( 177.1791022559528983, 56.75747545832872731, -14.00000000000006395 ) ) ;
#11958 = ORIENTED_EDGE ( 'NONE', *, *, #13146, .F. ) ;
#11959 = EDGE_CURVE ( 'NONE', #19623, #2860, #2053, .T. ) ;
#11960 = ORIENTED_EDGE ( 'NONE', *, *, #16529, .F. ) ;
#11961 = EDGE_CURVE ( 'NONE', #20547, #5368, #11576, .T. ) ;
#11962 = CARTESIAN_POINT ( 'NONE',  ( -20.18890516563201487, 67.16713051729674078, -2.731108915583016383 ) ) ;
#11963 = CIRCLE ( 'NONE', #14686, 2.499999999999997780 ) ;
#11964 = ORIENTED_EDGE ( 'NONE', *, *, #15084, .T. ) ;
#11965 = DIRECTION ( 'NONE',  ( 0.5000000000000054401, -0.8660254037844354880, 0.000000000000000000 ) ) ;
#11966 = PLANE ( 'NONE',  #3789 ) ;
#11967 = CARTESIAN_POINT ( 'NONE',  ( -26.07892689538028819, 45.11091634825275776, -7.401594269996666142 ) ) ;
#11968 = DIRECTION ( 'NONE',  ( -0.5000000000000047740, 0.8660254037844358210, 0.000000000000000000 ) ) ;
#11969 = B_SPLINE_CURVE_WITH_KNOTS ( 'NONE', 3,
 ( #1488, #2082, #11726, #19769 ),
 .UNSPECIFIED., .F., .F.,
 ( 4, 4 ),
 ( 0.000000000000000000, 0.001415162808320492545 ),
 .UNSPECIFIED. ) ;
#11970 = VERTEX_POINT ( 'NONE', #15215 ) ;
#11971 = DIRECTION ( 'NONE',  ( 0.000000000000000000, 1.000000000000000000, 3.469446951953589044E-16 ) ) ;
#11972 = DIRECTION ( 'NONE',  ( -0.3841106397986904786, 0.6652991438591134843, -0.6401843996644803747 ) ) ;
#11974 = ORIENTED_EDGE ( 'NONE', *, *, #1765, .T. ) ;
#11973 = ORIENTED_EDGE ( 'NONE', *, *, #14435, .T. ) ;
#11975 = AXIS2_PLACEMENT_3D ( 'NONE', #14304, #20739, #6207 ) ;
#11976 = CARTESIAN_POINT ( 'NONE',  ( 58.58539060705097512, 85.49268159961985702, -12.94168883615076560 ) ) ;
#11977 = VERTEX_POINT ( 'NONE', #13612 ) ;
#11978 = VERTEX_POINT ( 'NONE', #780 ) ;
#11979 = ORIENTED_EDGE ( 'NONE', *, *, #9132, .T. ) ;
#11980 = DIRECTION ( 'NONE',  ( 0.000000000000000000, -0.000000000000000000, -1.000000000000000000 ) ) ;
#11981 = CARTESIAN_POINT ( 'NONE',  ( -31.74999999999995737, 0.000000000000000000, 0.000000000000000000 ) ) ;
#11982 = EDGE_CURVE ( 'NONE', #14131, #16845, #19948, .T. ) ;
#11983 = ORIENTED_EDGE ( 'NONE', *, *, #16091, .F. ) ;
#11984 = EDGE_CURVE ( 'NONE', #18967, #206, #16571, .T. ) ;
#11985 = DIRECTION ( 'NONE',  ( 0.9949159024423659403, 0.000000000000000000, 0.1007092203688055299 ) ) ;
#11986 = CARTESIAN_POINT ( 'NONE',  ( 218.6693954511002858, 37.45238122438549055, -11.49787972461428964 ) ) ;
#11987 = CARTESIAN_POINT ( 'NONE',  ( 220.2899471553721753, 34.67552814235484959, -10.49174204642378605 ) ) ;
#11988 = VECTOR ( 'NONE', #20572, 1000.000000000000227 ) ;
#11989 = CARTESIAN_POINT ( 'NONE',  ( 221.7231637720595074, 32.81097251334476539, -16.48323849494068227 ) ) ;
#11990 = VECTOR ( 'NONE', #3821, 1000.000000000000000 ) ;
#11991 = ADVANCED_FACE ( 'NONE', ( #466 ), #16682, .F. ) ;
#11992 = DIRECTION ( 'NONE',  ( -0.7071067811865489050, 4.906538933386750403E-18, 0.7071067811865460184 ) ) ;
#11993 = DIRECTION ( 'NONE',  ( -0.2483788854152947367, -0.1434016163555419388, 0.9579895123154918979 ) ) ;
#11994 = DIRECTION ( 'NONE',  ( 0.000000000000000000, 0.7332630167743394711, -0.6799451067777418922 ) ) ;
#11995 = ORIENTED_EDGE ( 'NONE', *, *, #10239, .T. ) ;
#11996 = CARTESIAN_POINT ( 'NONE',  ( 216.3916581709072489, 15.88978658501442887, -14.00519583319098871 ) ) ;
#11997 = LINE ( 'NONE', #10270, #7567 ) ;
#11998 = DIRECTION ( 'NONE',  ( 0.8660254037844355990, 0.5000000000000054401, 0.000000000000000000 ) ) ;
#11999 = EDGE_LOOP ( 'NONE', ( #8444, #3771, #11517 ) ) ;
#12001 = EDGE_CURVE ( 'NONE', #9686, #2725, #11252, .T. ) ;
#12000 = FACE_OUTER_BOUND ( 'NONE', #14761, .T. ) ;
#12002 = VERTEX_POINT ( 'NONE', #13394 ) ;
#12003 = DIRECTION ( 'NONE',  ( 0.000000000000000000, 1.000000000000000000, -0.000000000000000000 ) ) ;
#12004 = CARTESIAN_POINT ( 'NONE',  ( 78.99950773051419617, 54.06482698700312284, -5.421535311907622834 ) ) ;
#12005 = EDGE_CURVE ( 'NONE', #14525, #15887, #1222, .T. ) ;
#12006 = EDGE_LOOP ( 'NONE', ( #15485, #7043, #4954, #5855 ) ) ;
#12007 = DIRECTION ( 'NONE',  ( 0.000000000000000000, 0.000000000000000000, 1.000000000000000000 ) ) ;
#12008 = CARTESIAN_POINT ( 'NONE',  ( 206.2111997916997552, 10.34978999605213268, -14.00000000000005507 ) ) ;
#12009 = VERTEX_POINT ( 'NONE', #8396 ) ;
#12010 = CARTESIAN_POINT ( 'NONE',  ( 75.54027896286939381, 52.67632256924044754, -8.347856068937160146 ) ) ;
#12011 = CARTESIAN_POINT ( 'NONE',  ( -17.04272031725003700, 79.99998834348832588, -12.47960036978351539 ) ) ;
#12012 = DIRECTION ( 'NONE',  ( -0.1997192025788092351, -0.1153079353712145594, 0.9730448705798270259 ) ) ;
#12013 = CARTESIAN_POINT ( 'NONE',  ( 189.5662401447910383, 15.47848971103284477, -19.61257667712936126 ) ) ;
#12014 = ADVANCED_FACE ( 'NONE', ( #361 ), #19844, .F. ) ;
#12015 = ADVANCED_FACE ( 'NONE', ( #14034 ), #3456, .F. ) ;
#12016 = DIRECTION ( 'NONE',  ( -0.8660254037844361541, -0.5000000000000045519, 5.976026924694054558E-17 ) ) ;
#12017 = VECTOR ( 'NONE', #10741, 1000.000000000000114 ) ;
#12018 = DIRECTION ( 'NONE',  ( -0.8660254037844354880, -0.5000000000000055511, 0.000000000000000000 ) ) ;
#12019 = DIRECTION ( 'NONE',  ( 0.000000000000000000, 6.938893903907177533E-18, 1.000000000000000000 ) ) ;
#12020 = ORIENTED_EDGE ( 'NONE', *, *, #3860, .T. ) ;
#12022 = EDGE_CURVE ( 'NONE', #4848, #437, #10944, .T. ) ;
#12021 = CYLINDRICAL_SURFACE ( 'NONE', #7113, 12.47473710546057646 ) ;
#12023 = DIRECTION ( 'NONE',  ( 0.5000000000000051070, -0.8660254037844358210, 0.000000000000000000 ) ) ;
#12024 = CARTESIAN_POINT ( 'NONE',  ( 196.2703485803101842, 4.433426968998789519, -19.44895743303468905 ) ) ;
#12025 = CARTESIAN_POINT ( 'NONE',  ( -14.69781867356227245, 79.99997331865614569, -12.46740305798945592 ) ) ;
#12027 = ORIENTED_EDGE ( 'NONE', *, *, #13810, .T. ) ;
#12026 = ORIENTED_EDGE ( 'NONE', *, *, #3529, .F. ) ;
#12028 = ORIENTED_EDGE ( 'NONE', *, *, #19792, .T. ) ;
#12029 = ORIENTED_EDGE ( 'NONE', *, *, #624, .F. ) ;
#12030 = LINE ( 'NONE', #793, #15651 ) ;
#12031 = DIRECTION ( 'NONE',  ( -0.8660254037844363761, -0.5000000000000043299, 6.872020471724002955E-17 ) ) ;
#12032 = FACE_OUTER_BOUND ( 'NONE', #3238, .T. ) ;
#12033 = EDGE_CURVE ( 'NONE', #17073, #8802, #20266, .T. ) ;
#12034 = CARTESIAN_POINT ( 'NONE',  ( 74.47592707218369412, 73.05594451708931558, -24.62326922035613208 ) ) ;
#12035 = VECTOR ( 'NONE', #1874, 1000.000000000000000 ) ;
#12036 = CARTESIAN_POINT ( 'NONE',  ( -28.14271859785574748, 6.485482021666785890, 3.095587321074997789 ) ) ;
#12037 = CARTESIAN_POINT ( 'NONE',  ( -15.99999999999999289, 80.00000000000000000, -4.999999999999989342 ) ) ;
#12038 = VERTEX_POINT ( 'NONE', #7648 ) ;
#12039 = CARTESIAN_POINT ( 'NONE',  ( 80.21267746518212505, 56.48438466791053258, -22.35508466618705015 ) ) ;
#12040 = PLANE ( 'NONE',  #15914 ) ;
#12041 = ORIENTED_EDGE ( 'NONE', *, *, #11663, .T. ) ;
#12042 = CARTESIAN_POINT ( 'NONE',  ( 202.4761207370255818, 24.94531058701918980, -15.49001580682321233 ) ) ;
#12043 = DIRECTION ( 'NONE',  ( 0.000000000000000000, 1.000000000000000000, 0.000000000000000000 ) ) ;
#12044 = CARTESIAN_POINT ( 'NONE',  ( 215.7779675912125867, 15.87316596037559968, -12.64773574313060678 ) ) ;
#12045 = PLANE ( 'NONE',  #4726 ) ;
#12046 = CARTESIAN_POINT ( 'NONE',  ( 202.1791022559531541, 13.45620526910691694, 0.9999999999999232836 ) ) ;
#12047 = AXIS2_PLACEMENT_3D ( 'NONE', #4781, #17516, #14454 ) ;
#12049 = ORIENTED_EDGE ( 'NONE', *, *, #7381, .F. ) ;
#12048 = ORIENTED_EDGE ( 'NONE', *, *, #14090, .F. ) ;
#12050 = B_SPLINE_CURVE_WITH_KNOTS ( 'NONE', 3,
 ( #11, #19397, #11766, #1806 ),
 .UNSPECIFIED., .F., .F.,
 ( 4, 4 ),
 ( 2.736592200873451967E-07, 0.0005857620149597038113 ),
 .UNSPECIFIED. ) ;
#12051 = ORIENTED_EDGE ( 'NONE', *, *, #18228, .F. ) ;
#12052 = VECTOR ( 'NONE', #15599, 1000.000000000000227 ) ;
#12053 = EDGE_LOOP ( 'NONE', ( #16727, #99, #18551, #7739 ) ) ;
#12054 = PLANE ( 'NONE',  #17319 ) ;
#12055 = CARTESIAN_POINT ( 'NONE',  ( 216.3683575532813848, 33.19538101841231992, -14.00000000000004441 ) ) ;
#12056 = ORIENTED_EDGE ( 'NONE', *, *, #10911, .F. ) ;
#12057 = ORIENTED_EDGE ( 'NONE', *, *, #16335, .F. ) ;
#12058 = CARTESIAN_POINT ( 'NONE',  ( 80.22357501274980507, 59.31776527496312923, -0.7804667811256712495 ) ) ;
#12059 = DIRECTION ( 'NONE',  ( 0.5000000000000045519, -0.8660254037844360431, 0.000000000000000000 ) ) ;
#12060 = DIRECTION ( 'NONE',  ( 0.000000000000000000, -1.000000000000000000, 0.000000000000000000 ) ) ;
#12061 = DIRECTION ( 'NONE',  ( 0.000000000000000000, 0.6847449705900804373, -0.7287827695902187042 ) ) ;
#12062 = DIRECTION ( 'NONE',  ( 0.8660254037844380415, 0.5000000000000014433, 0.000000000000000000 ) ) ;
#12063 = AXIS2_PLACEMENT_3D ( 'NONE', #17814, #6873, #14967 ) ;
#12064 = AXIS2_PLACEMENT_3D ( 'NONE', #8351, #6969, #8452 ) ;
#12065 = DIRECTION ( 'NONE',  ( -0.8660254037844363761, -0.5000000000000037748, 0.000000000000000000 ) ) ;
#12066 = CARTESIAN_POINT ( 'NONE',  ( 4.000000000000000000, 0.000000000000000000, 0.000000000000000000 ) ) ;
#12067 = CARTESIAN_POINT ( 'NONE',  ( -14.28506451248627940, 45.59460031122257107, -12.38656090347159022 ) ) ;
#12068 = DIRECTION ( 'NONE',  ( 0.6048098792058420603, 0.000000000000000000, -0.7963698952214447457 ) ) ;
#12069 = ORIENTED_EDGE ( 'NONE', *, *, #4038, .T. ) ;
#12070 = CARTESIAN_POINT ( 'NONE',  ( -83.06735915341819521, 143.8768865042907521, 44.53282986889873740 ) ) ;
#12071 = DIRECTION ( 'NONE',  ( 0.7500000000000013323, 0.4330127018922261817, 0.4999999999999918954 ) ) ;
#12072 = EDGE_CURVE ( 'NONE', #5803, #15680, #7542, .T. ) ;
#12074 = ORIENTED_EDGE ( 'NONE', *, *, #1626, .T. ) ;
#12073 = EDGE_LOOP ( 'NONE', ( #5848, #2847 ) ) ;
#12075 = VECTOR ( 'NONE', #10179, 1000.000000000000000 ) ;
#12076 = CARTESIAN_POINT ( 'NONE',  ( 62.41741185223617805, 78.28105863300197598, -15.10370911918632331 ) ) ;
#12077 = ORIENTED_EDGE ( 'NONE', *, *, #8175, .F. ) ;
#12078 = AXIS2_PLACEMENT_3D ( 'NONE', #7267, #2203, #5252 ) ;
#12079 = DIRECTION ( 'NONE',  ( -1.000000000000000000, 0.000000000000000000, 0.000000000000000000 ) ) ;
#12080 = CARTESIAN_POINT ( 'NONE',  ( 208.0983737146324870, 5.661548828456886895, -14.00000000000005507 ) ) ;
#12081 = EDGE_LOOP ( 'NONE', ( #13624, #11061, #16911, #5012 ) ) ;
#12082 = ORIENTED_EDGE ( 'NONE', *, *, #11156, .F. ) ;
#12083 = CARTESIAN_POINT ( 'NONE',  ( 227.5312376355471145, 39.64027283883993391, -14.00000000000005507 ) ) ;
#12085 = ADVANCED_FACE ( 'NONE', ( #5628, #4269 ), #15830, .F. ) ;
#12084 = CARTESIAN_POINT ( 'NONE',  ( 200.2585560139914378, -0.5099779577875940273, -20.52105855319921801 ) ) ;
#12086 = LINE ( 'NONE', #20342, #17404 ) ;
#12087 = CARTESIAN_POINT ( 'NONE',  ( -13.48328391324397657, 19.43205798116640537, 12.24715376271861800 ) ) ;
#12088 = AXIS2_PLACEMENT_3D ( 'NONE', #3967, #13518, #7138 ) ;
#12089 = DIRECTION ( 'NONE',  ( -0.1348983855785064190, 0.2336508576809882276, -0.9629172873478029082 ) ) ;
#12090 = CARTESIAN_POINT ( 'NONE',  ( 72.49529059433407951, 198.3908428320658288, 11.00000000000001066 ) ) ;
#12091 = AXIS2_PLACEMENT_3D ( 'NONE', #1589, #15813, #12423 ) ;
#12092 = CARTESIAN_POINT ( 'NONE',  ( 221.0007431456517395, 33.44439337337441032, -11.10922658182128764 ) ) ;
#12093 = EDGE_CURVE ( 'NONE', #12773, #18967, #5842, .T. ) ;
#12094 = CARTESIAN_POINT ( 'NONE',  ( -28.02004479723489894, 75.03053098945940746, 3.432994178266289165 ) ) ;
#12095 = DIRECTION ( 'NONE',  ( 0.1348983855785130803, -0.2336508576809998017, -0.9629172873477991335 ) ) ;
#12096 = CARTESIAN_POINT ( 'NONE',  ( 226.6211368133091923, 39.11482588413117867, -14.00000000000005507 ) ) ;
#12097 = EDGE_CURVE ( 'NONE', #9868, #330, #1480, .T. ) ;
#12098 = VERTEX_POINT ( 'NONE', #4165 ) ;
#12099 = CARTESIAN_POINT ( 'NONE',  ( -3.768439905627497755, 65.75000000000002842, 3.993547312438780583 ) ) ;
#12100 = ORIENTED_EDGE ( 'NONE', *, *, #6561, .F. ) ;
#12101 = CYLINDRICAL_SURFACE ( 'NONE', #13903, 12.47473710546057646 ) ;
#12102 = CARTESIAN_POINT ( 'NONE',  ( 76.86472363869455648, 54.45620830782070954, -4.878812238591026862 ) ) ;
#12103 = ADVANCED_FACE ( 'NONE', ( #10616 ), #20472, .F. ) ;
#12104 = VECTOR ( 'NONE', #2106, 999.9999999999998863 ) ;
#12105 = DIRECTION ( 'NONE',  ( -0.4977263686445478896, 0.8620873587591040277, 0.09525674686689167281 ) ) ;
#12106 = AXIS2_PLACEMENT_3D ( 'NONE', #13956, #9156, #2717 ) ;
#12107 = B_SPLINE_CURVE_WITH_KNOTS ( 'NONE', 3,
 ( #5364, #4744, #4851, #16204 ),
 .UNSPECIFIED., .F., .F.,
 ( 4, 4 ),
 ( 7.900540974747862941E-05, 0.0007516562018010966269 ),
 .UNSPECIFIED. ) ;
#12108 = LINE ( 'NONE', #15728, #13685 ) ;
#12109 = ORIENTED_EDGE ( 'NONE', *, *, #20343, .F. ) ;
#12110 = CARTESIAN_POINT ( 'NONE',  ( 75.08392619713679039, 52.07086927207439686, -10.97824920096100065 ) ) ;
#12111 = CARTESIAN_POINT ( 'NONE',  ( 229.1914409901575880, 36.76471627775831763, -11.94979443502199956 ) ) ;
#12112 = DIRECTION ( 'NONE',  ( -0.8660254037844360431, -0.5000000000000044409, 5.976026924694052093E-17 ) ) ;
#12113 = FACE_OUTER_BOUND ( 'NONE', #6920, .T. ) ;
#12114 = EDGE_CURVE ( 'NONE', #14274, #3298, #7752, .T. ) ;
#12115 = EDGE_LOOP ( 'NONE', ( #15433, #5040, #17822, #1168 ) ) ;
#12116 = CARTESIAN_POINT ( 'NONE',  ( 218.0676437282319569, 37.01116419957239856, -10.52647298641110396 ) ) ;
#12117 = EDGE_CURVE ( 'NONE', #10224, #10441, #14154, .T. ) ;
#12118 = DIRECTION ( 'NONE',  ( -0.000000000000000000, 1.000000000000000000, -0.000000000000000000 ) ) ;
#12119 = AXIS2_PLACEMENT_3D ( 'NONE', #1344, #20733, #379 ) ;
#12120 = FACE_OUTER_BOUND ( 'NONE', #10456, .T. ) ;
#12121 = PRODUCT ( 'Drill Bit Indexing Pin', 'Drill Bit Indexing Pin', '', ( #16770 ) ) ;
#12122 =( NAMED_UNIT ( * ) SI_UNIT ( $, .STERADIAN. ) SOLID_ANGLE_UNIT ( ) );
#12124 = CARTESIAN_POINT ( 'NONE',  ( 10.49211908931699178, -24.14213562373095456, -5.000000000000000000 ) ) ;
#12123 = CIRCLE ( 'NONE', #9729, 12.47473710546057823 ) ;
#12125 = DIRECTION ( 'NONE',  ( -0.8660254037844359321, -0.5000000000000045519, 5.976026924694053325E-17 ) ) ;
#12126 = DIRECTION ( 'NONE',  ( -0.5000000000000049960, 0.8660254037844358210, 0.000000000000000000 ) ) ;
#12127 = EDGE_CURVE ( 'NONE', #17881, #8085, #5943, .T. ) ;
#12129 = ORIENTED_EDGE ( 'NONE', *, *, #10561, .T. ) ;
#12128 = EDGE_LOOP ( 'NONE', ( #5203, #13751, #15534, #10890 ) ) ;
#12130 = EDGE_CURVE ( 'NONE', #5457, #14274, #15421, .T. ) ;
#12131 = LINE ( 'NONE', #16582, #5829 ) ;
#12132 = CARTESIAN_POINT ( 'NONE',  ( 28.00000000000001066, 64.25000000000000000, 1.479896280015810639 ) ) ;
#12133 = ORIENTED_EDGE ( 'NONE', *, *, #422, .T. ) ;
#12134 = CARTESIAN_POINT ( 'NONE',  ( 226.0801508759606975, 43.13309472369712694, -12.92165662794185543 ) ) ;
#12135 = CARTESIAN_POINT ( 'NONE',  ( 68.52857421331229659, 77.79673560728132031, -22.80503257933564853 ) ) ;
#12136 = COLOUR_RGB ( '',0.7921568627450980005, 0.8196078431372548767, 0.9333333333333333481 ) ;
#12137 = CARTESIAN_POINT ( 'NONE',  ( -27.65088713606887438, 9.446972530103739274, 4.576488380515961296 ) ) ;
#12138 = SHAPE_REPRESENTATION_RELATIONSHIP ( 'NONE' , 'NONE' ,  #1796, #7815 ) ;
#12139 = DIRECTION ( 'NONE',  ( 0.8296432542242747621, 0.4789947561577490021, -0.2868032327110942581 ) ) ;
#12140 = EDGE_CURVE ( 'NONE', #184, #16451, #5488, .T. ) ;
#12141 = ORIENTED_EDGE ( 'NONE', *, *, #1252, .T. ) ;
#12142 = CARTESIAN_POINT ( 'NONE',  ( 82.89519626194027069, 61.38757715954039185, -25.23100993346370302 ) ) ;
#12143 = CARTESIAN_POINT ( 'NONE',  ( 217.4610193877672941, 9.421868901786666584, -7.448751785191543462 ) ) ;
#12144 = ORIENTED_EDGE ( 'NONE', *, *, #17600, .F. ) ;
#12145 = B_SPLINE_CURVE_WITH_KNOTS ( 'NONE', 3,
 ( #20822, #12892, #8088, #6297, #18073, #17873, #4717, #9687, #12789, #16181, #3137, #11495, #3338, #14495, #15978, #20921, #11188, #9888, #14394, #14599, #9787, #1649, #16272, #6601, #9582, #1752, #16081, #19249, #6705, #8199 ),
 .UNSPECIFIED., .F., .F.,
 ( 4, 2, 2, 2, 2, 2, 2, 2, 2, 2, 2, 2, 2, 2, 4 ),
 ( 0.007829808997192468090, 0.008808290957735770768, 0.009297531938007422975, 0.009786772918279073447, 0.01027601389855072565, 0.01076525487882237613, 0.01125449585909402833, 0.01174373683936567880, 0.01223297781963733101, 0.01272221879990898322, 0.01321145978018063369, 0.01370070076045228416, 0.01467918272099555388, 0.01516842370126719915, 0.01565766468153884441 ),
 .UNSPECIFIED. ) ;
#12146 = CARTESIAN_POINT ( 'NONE',  ( 205.5965122587965084, 9.994899983462953941, -14.00000000000005507 ) ) ;
#12147 = CARTESIAN_POINT ( 'NONE',  ( 195.8472345282168874, 4.366151861308305016, -18.11117897393217646 ) ) ;
#12148 = B_SPLINE_CURVE_WITH_KNOTS ( 'NONE', 3,
 ( #4511, #17340, #14487, #10974 ),
 .UNSPECIFIED., .F., .F.,
 ( 4, 4 ),
 ( 5.953779341697503242E-07, 0.0004526486197140639671 ),
 .UNSPECIFIED. ) ;
#12149 = EDGE_CURVE ( 'NONE', #385, #1597, #5516, .T. ) ;
#12150 = B_SPLINE_CURVE_WITH_KNOTS ( 'NONE', 3,
 ( #17469, #13986, #9385, #12395 ),
 .UNSPECIFIED., .F., .F.,
 ( 4, 4 ),
 ( 5.481513501348629134E-07, 0.0006731989433939361729 ),
 .UNSPECIFIED. ) ;
#12151 = DIRECTION ( 'NONE',  ( 0.4953429730181675983, -0.8579591964396817705, -0.1361666490962400167 ) ) ;
#12152 = CARTESIAN_POINT ( 'NONE',  ( 164.5049095375683521, 9.025508037334198264, -14.00000000000000355 ) ) ;
#12153 = FACE_OUTER_BOUND ( 'NONE', #10393, .T. ) ;
#12154 = CIRCLE ( 'NONE', #11801, 3.902363844300875240 ) ;
#12155 = ORIENTED_EDGE ( 'NONE', *, *, #10284, .T. ) ;
#12156 = ORIENTED_EDGE ( 'NONE', *, *, #8051, .T. ) ;
#12157 = CARTESIAN_POINT ( 'NONE',  ( 205.0662616026534693, 10.91332106064940888, -14.00000000000005507 ) ) ;
#12158 = ADVANCED_FACE ( 'NONE', ( #13816 ), #775, .T. ) ;
#12159 = ORIENTED_EDGE ( 'NONE', *, *, #11068, .T. ) ;
#12160 = ORIENTED_EDGE ( 'NONE', *, *, #10002, .T. ) ;
#12161 = CARTESIAN_POINT ( 'NONE',  ( 30.10683012259193703, -10.00000000000000000, 0.000000000000000000 ) ) ;
#12162 = CARTESIAN_POINT ( 'NONE',  ( 205.5965122587965084, 9.994899983462953941, -14.00000000000005507 ) ) ;
#12163 = CARTESIAN_POINT ( 'NONE',  ( 219.7265866098479989, 34.13779084175865819, -9.834987871251062330 ) ) ;
#12164 = LINE ( 'NONE', #7268, #7631 ) ;
#12165 = CARTESIAN_POINT ( 'NONE',  ( -17.40260810207333719, 71.39595272406131699, -4.812026853405401816 ) ) ;
#12166 = ORIENTED_EDGE ( 'NONE', *, *, #10300, .T. ) ;
#12167 = AXIS2_PLACEMENT_3D ( 'NONE', #7072, #8561, #15059 ) ;
#12168 = B_SPLINE_CURVE_WITH_KNOTS ( 'NONE', 3,
 ( #5190, #6778, #16149, #13272 ),
 .UNSPECIFIED., .F., .F.,
 ( 4, 4 ),
 ( 0.0001032701082515755423, 0.0009572558462284362375 ),
 .UNSPECIFIED. ) ;
#12169 = DIRECTION ( 'NONE',  ( 5.175391130484829193E-17, 2.988013462347053780E-17, 1.000000000000000000 ) ) ;
#12170 = DIRECTION ( 'NONE',  ( -0.5000000000000008882, 0.8660254037844381525, 0.000000000000000000 ) ) ;
#12171 = CARTESIAN_POINT ( 'NONE',  ( -23.40647577390874545, 45.06233805004389836, -10.07534141557004226 ) ) ;
#12172 = PLANE ( 'NONE',  #1454 ) ;
#12173 = LINE ( 'NONE', #8976, #16606 ) ;
#12174 = CARTESIAN_POINT ( 'NONE',  ( 63.15554463217812042, 234.5677573683057062, -8.999999999999973355 ) ) ;
#12176 = ORIENTED_EDGE ( 'NONE', *, *, #12022, .T. ) ;
#12175 = ORIENTED_EDGE ( 'NONE', *, *, #20287, .F. ) ;
#12177 = DIRECTION ( 'NONE',  ( -0.4999999999999995004, 0.8660254037844390407, 0.000000000000000000 ) ) ;
#12178 = CARTESIAN_POINT ( 'NONE',  ( 54.25075523830079760, 77.99786835657231165, -12.14770500197372627 ) ) ;
#12179 = VERTEX_POINT ( 'NONE', #10827 ) ;
#12180 = EDGE_LOOP ( 'NONE', ( #18941, #11690, #7661, #19069, #1569 ) ) ;
#12181 = AXIS2_PLACEMENT_3D ( 'NONE', #19356, #4418, #8001 ) ;
#12182 = CARTESIAN_POINT ( 'NONE',  ( 227.5454127698698130, 40.59518667705200556, -17.81526153211078523 ) ) ;
#12183 = VECTOR ( 'NONE', #15452, 1000.000000000000000 ) ;
#12184 = CARTESIAN_POINT ( 'NONE',  ( 10.49211908931699178, 0.000000000000000000, 5.999999999999998224 ) ) ;
#12185 = AXIS2_PLACEMENT_3D ( 'NONE', #8424, #3150, #5142 ) ;
#12186 = ORIENTED_EDGE ( 'NONE', *, *, #5211, .F. ) ;
#12187 = ORIENTED_EDGE ( 'NONE', *, *, #2019, .F. ) ;
#12188 = DIRECTION ( 'NONE',  ( -0.5000000000000042188, 0.8660254037844362651, 0.000000000000000000 ) ) ;
#12189 = EDGE_LOOP ( 'NONE', ( #11162, #17505, #15759, #19715 ) ) ;
#12190 = VECTOR ( 'NONE', #14782, 1000.000000000000114 ) ;
#12191 = LINE ( 'NONE', #2550, #4994 ) ;
#12192 = DIRECTION ( 'NONE',  ( 0.8660254037844380415, 0.5000000000000014433, 0.000000000000000000 ) ) ;
#12193 = ADVANCED_FACE ( 'NONE', ( #15735 ), #14254, .T. ) ;
#12194 = CARTESIAN_POINT ( 'NONE',  ( -11.51383524490820420, 17.33161812738734753, 11.66803293973013389 ) ) ;
#12195 =( BOUNDED_CURVE ( )  B_SPLINE_CURVE ( 3, ( #6237, #20458, #5925, #17183 ),
 .UNSPECIFIED., .F., .F. ) 
 B_SPLINE_CURVE_WITH_KNOTS ( ( 4, 4 ),
 ( 3.141592653589793116, 4.511031059594355241 ),
 .UNSPECIFIED. ) 
 CURVE ( )  GEOMETRIC_REPRESENTATION_ITEM ( )  RATIONAL_B_SPLINE_CURVE ( ( 1.000000000000000000, 0.8497311128276563430, 0.8497311128276563430, 1.000000000000000000 ) ) 
 REPRESENTATION_ITEM ( '' )  );
#12196 = ORIENTED_EDGE ( 'NONE', *, *, #8743, .F. ) ;
#12197 = CARTESIAN_POINT ( 'NONE',  ( 61.55523633728010680, 134.3395726428436774, -12.50000000000000000 ) ) ;
#12198 = CARTESIAN_POINT ( 'NONE',  ( 34.99529059433363898, 263.3427481158985302, -5.999999999999973355 ) ) ;
#12199 = CARTESIAN_POINT ( 'NONE',  ( 4.000000000000000000, 4.131365146527188963E-15, 3.047499999999999432 ) ) ;
#12200 = CIRCLE ( 'NONE', #18, 4.171999999999999709 ) ;
#12201 = ORIENTED_EDGE ( 'NONE', *, *, #10376, .F. ) ;
#12202 = CARTESIAN_POINT ( 'NONE',  ( -28.45830647201975694, 79.08610913873366144, 1.260722419664553673 ) ) ;
#12203 = VECTOR ( 'NONE', #15330, 1000.000000000000114 ) ;
#12204 = CARTESIAN_POINT ( 'NONE',  ( 202.1791022559531541, 13.45620526910691694, -14.00000000000008527 ) ) ;
#12205 = DIRECTION ( 'NONE',  ( 0.000000000000000000, 0.000000000000000000, -1.000000000000000000 ) ) ;
#12206 = ORIENTED_EDGE ( 'NONE', *, *, #2629, .F. ) ;
#12207 = CARTESIAN_POINT ( 'NONE',  ( 62.36389338619030553, 105.9389375482328006, -29.00000000000000000 ) ) ;
#12208 = EDGE_CURVE ( 'NONE', #1834, #20270, #18372, .T. ) ;
#12209 = VERTEX_POINT ( 'NONE', #8159 ) ;
#12210 = CARTESIAN_POINT ( 'NONE',  ( 92.15025355475009405, 206.8071376747316492, 11.00000000000001066 ) ) ;
#12211 = CARTESIAN_POINT ( 'NONE',  ( 196.9187795697884269, 4.984808679508447860, -7.425127016398286983 ) ) ;
#12212 = CIRCLE ( 'NONE', #10490, 7.155882939242646401 ) ;
#12213 = APPLICATION_PROTOCOL_DEFINITION ( 'draft international standard', 'automotive_design', 1998, #5921 ) ;
#12214 = VECTOR ( 'NONE', #31, 1000.000000000000000 ) ;
#12215 = EDGE_CURVE ( 'NONE', #2199, #5956, #8796, .T. ) ;
#12216 = CIRCLE ( 'NONE', #8830, 4.999999999999995559 ) ;
#12217 = CARTESIAN_POINT ( 'NONE',  ( 58.37797649651341203, 276.8427481158987007, 1.000000000000017097 ) ) ;
#12218 = ORIENTED_EDGE ( 'NONE', *, *, #3575, .T. ) ;
#12219 =( LENGTH_UNIT ( ) NAMED_UNIT ( * ) SI_UNIT ( .MILLI., .METRE. ) );
#12220 = EDGE_CURVE ( 'NONE', #9607, #15521, #11050, .T. ) ;
#12221 = DIRECTION ( 'NONE',  ( 0.5000000000000051070, -0.8660254037844359321, 0.000000000000000000 ) ) ;
#12222 = LINE ( 'NONE', #4266, #14407 ) ;
#12223 = CARTESIAN_POINT ( 'NONE',  ( 205.5965122587965084, 9.994899983462953941, -14.00000000000005507 ) ) ;
#12224 = CIRCLE ( 'NONE', #11873, 1.499999999999993783 ) ;
#12225 = DIRECTION ( 'NONE',  ( 0.3535533905932770060, -0.6123724356957921389, 0.7071067811865480168 ) ) ;
#12226 = CIRCLE ( 'NONE', #9491, 3.461721407990061117 ) ;
#12227 = FACE_OUTER_BOUND ( 'NONE', #7921, .T. ) ;
#12228 = DIRECTION ( 'NONE',  ( 0.1348983855785064190, -0.2336508576809882831, 0.9629172873478027972 ) ) ;
#12229 = EDGE_LOOP ( 'NONE', ( #17533, #3376, #6062, #13729, #11791 ) ) ;
#12230 = VECTOR ( 'NONE', #11053, 1000.000000000000227 ) ;
#12231 = VECTOR ( 'NONE', #19565, 1000.000000000000114 ) ;
#12232 = CARTESIAN_POINT ( 'NONE',  ( 0.000000000000000000, 5.000000000000000000, -30.00000000000000000 ) ) ;
#12233 = CARTESIAN_POINT ( 'NONE',  ( 228.9802228740807948, 38.11002267734541959, -16.98332657222556108 ) ) ;
#12234 = AXIS2_PLACEMENT_3D ( 'NONE', #2827, #20818, #4516 ) ;
#12235 = PRODUCT_RELATED_PRODUCT_CATEGORY ( 'part', '', ( #8552 ) ) ;
#12236 = CARTESIAN_POINT ( 'NONE',  ( -20.40277896402405133, 18.53029315133363752, 3.430876175762952673 ) ) ;
#12237 = DIRECTION ( 'NONE',  ( 0.5000000000000058842, -0.8660254037844352659, 0.000000000000000000 ) ) ;
#12238 = EDGE_CURVE ( 'NONE', #9425, #13939, #3803, .T. ) ;
#12240 = ORIENTED_EDGE ( 'NONE', *, *, #91, .T. ) ;
#12239 = EDGE_LOOP ( 'NONE', ( #6691, #8679, #19164, #7609 ) ) ;
#12241 = ORIENTED_EDGE ( 'NONE', *, *, #7406, .T. ) ;
#12242 = ORIENTED_EDGE ( 'NONE', *, *, #3134, .T. ) ;
#12243 = PLANE ( 'NONE',  #12933 ) ;
#12244 = FILL_AREA_STYLE ('',( #17216 ) ) ;
#12245 = ORIENTED_EDGE ( 'NONE', *, *, #12140, .T. ) ;
#12246 = ADVANCED_FACE ( 'NONE', ( #19211 ), #9550, .T. ) ;
#12247 = TOROIDAL_SURFACE ( 'NONE', #5789, 6.500000000000000888, 1.500000000000000000 ) ;
#12248 = DIRECTION ( 'NONE',  ( 0.8660254037844359321, 0.5000000000000046629, 0.000000000000000000 ) ) ;
#12249 = CARTESIAN_POINT ( 'NONE',  ( 218.2609288254238322, 38.39580918011897381, -14.95362368770807748 ) ) ;
#12250 = ORIENTED_EDGE ( 'NONE', *, *, #2493, .T. ) ;
#12251 = AXIS2_PLACEMENT_3D ( 'NONE', #1821, #6671, #11572 ) ;
#12252 = AXIS2_PLACEMENT_3D ( 'NONE', #2068, #3965, #10414 ) ;
#12253 = DIRECTION ( 'NONE',  ( 0.8660254037844380415, 0.5000000000000014433, 0.000000000000000000 ) ) ;
#12254 = AXIS2_PLACEMENT_3D ( 'NONE', #5499, #5391, #20037 ) ;
#12255 = CARTESIAN_POINT ( 'NONE',  ( 218.3827643905817411, 38.39073589366585537, -12.52024606262105877 ) ) ;
#12256 = AXIS2_PLACEMENT_3D ( 'NONE', #6075, #9359, #17756 ) ;
#12257 = ADVANCED_FACE ( 'NONE', ( #3100 ), #6497, .T. ) ;
#12258 = EDGE_LOOP ( 'NONE', ( #15333, #12133, #347, #14898, #8698, #6017, #5979 ) ) ;
#12259 = CARTESIAN_POINT ( 'NONE',  ( 215.2800591377192916, 15.23167179936302240, -8.480087152951449880 ) ) ;
#12260 = CARTESIAN_POINT ( 'NONE',  ( 218.3339933646592499, 38.03331467906619423, -12.44819273571337703 ) ) ;
#12261 = LINE ( 'NONE', #17026, #12183 ) ;
#12262 = DIRECTION ( 'NONE',  ( -0.8660254037844360431, -0.5000000000000044409, 0.000000000000000000 ) ) ;
#12263 = CARTESIAN_POINT ( 'NONE',  ( 5.000000000000000000, 0.000000000000000000, 0.000000000000000000 ) ) ;
#12265 = ORIENTED_EDGE ( 'NONE', *, *, #15494, .T. ) ;
#12264 = VERTEX_POINT ( 'NONE', #15937 ) ;
#12266 = VERTEX_POINT ( 'NONE', #8263 ) ;
#12267 = CARTESIAN_POINT ( 'NONE',  ( 26.99999999999999645, 64.25000000000000000, -2.528164662410438357 ) ) ;
#12268 = AXIS2_PLACEMENT_3D ( 'NONE', #19741, #5209, #3949 ) ;
#12269 = EDGE_CURVE ( 'NONE', #16764, #20210, #9050, .T. ) ;
#12270 = AXIS2_PLACEMENT_3D ( 'NONE', #16731, #8562, #11857 ) ;
#12271 = VERTEX_POINT ( 'NONE', #20885 ) ;
#12272 = ORIENTED_EDGE ( 'NONE', *, *, #7420, .F. ) ;
#12273 = ORIENTED_EDGE ( 'NONE', *, *, #4632, .F. ) ;
#12274 = DIRECTION ( 'NONE',  ( 0.8660254037844377084, 0.5000000000000015543, 0.000000000000000000 ) ) ;
#12275 = CYLINDRICAL_SURFACE ( 'NONE', #6460, 6.500000000000000000 ) ;
#12276 = PLANE ( 'NONE',  #18841 ) ;
#12277 = EDGE_CURVE ( 'NONE', #4912, #9631, #17624, .T. ) ;
#12278 = CARTESIAN_POINT ( 'NONE',  ( 206.2111997916997552, 10.34978999605213623, -2.187257959407755248 ) ) ;
#12279 = CARTESIAN_POINT ( 'NONE',  ( 227.5678821218066901, 40.55626861788441317, -17.48830818005195908 ) ) ;
#12280 = EDGE_CURVE ( 'NONE', #14638, #18324, #8053, .T. ) ;
#12281 = ORIENTED_EDGE ( 'NONE', *, *, #14461, .T. ) ;
#12282 = ORIENTED_EDGE ( 'NONE', *, *, #18729, .T. ) ;
#12283 = VECTOR ( 'NONE', #988, 1000.000000000000114 ) ;
#12284 = DIRECTION ( 'NONE',  ( -0.5000000000000054401, 0.8660254037844354880, -0.000000000000000000 ) ) ;
#12285 = VECTOR ( 'NONE', #18349, 1000.000000000000000 ) ;
#12286 = EDGE_CURVE ( 'NONE', #18774, #9345, #7955, .T. ) ;
#12287 = ADVANCED_FACE ( 'NONE', ( #14460 ), #11459, .F. ) ;
#12288 = CARTESIAN_POINT ( 'NONE',  ( -15.31857793801784062, 45.63007274853293893, -12.48623160004378363 ) ) ;
#12289 = DIRECTION ( 'NONE',  ( 0.4999999999999997224, -0.8660254037844388186, 0.000000000000000000 ) ) ;
#12290 = DIRECTION ( 'NONE',  ( -1.000000000000000000, -0.000000000000000000, -0.000000000000000000 ) ) ;
#12291 = CARTESIAN_POINT ( 'NONE',  ( -31.74999999999995737, 4.898587196589412829E-16, -4.000000000000000000 ) ) ;
#12293 = ORIENTED_EDGE ( 'NONE', *, *, #11804, .T. ) ;
#12292 = ORIENTED_EDGE ( 'NONE', *, *, #618, .F. ) ;
#12294 = CYLINDRICAL_SURFACE ( 'NONE', #20001, 12.47473710546057646 ) ;
#12295 = FACE_OUTER_BOUND ( 'NONE', #15305, .T. ) ;
#12296 = ADVANCED_FACE ( 'NONE', ( #17934 ), #13289, .T. ) ;
#12297 = LINE ( 'NONE', #15792, #20582 ) ;
#12298 = ORIENTED_EDGE ( 'NONE', *, *, #3426, .F. ) ;
#12299 = ORIENTED_EDGE ( 'NONE', *, *, #20504, .T. ) ;
#12300 = EDGE_LOOP ( 'NONE', ( #12129, #13699, #6981, #12325, #14373, #9678 ) ) ;
#12301 = LINE ( 'NONE', #14633, #2779 ) ;
#12302 = FACE_OUTER_BOUND ( 'NONE', #6186, .T. ) ;
#12303 = CARTESIAN_POINT ( 'NONE',  ( 0.8775796894216562061, 57.25228208760839266, 0.3499516663593752464 ) ) ;
#12304 = CARTESIAN_POINT ( 'NONE',  ( 195.3173534746875930, 3.529175630622251258, -16.89203719259486647 ) ) ;
#12305 = VECTOR ( 'NONE', #18323, 1000.000000000000114 ) ;
#12306 = ORIENTED_EDGE ( 'NONE', *, *, #11536, .T. ) ;
#12307 = ORIENTED_EDGE ( 'NONE', *, *, #12582, .F. ) ;
#12308 = FACE_OUTER_BOUND ( 'NONE', #15169, .T. ) ;
#12309 = ORIENTED_EDGE ( 'NONE', *, *, #17154, .F. ) ;
#12310 = EDGE_CURVE ( 'NONE', #3963, #13939, #2986, .T. ) ;
#12311 = DIRECTION ( 'NONE',  ( -0.6123724356957914727, -0.3535533905932749521, -0.7071067811865495711 ) ) ;
#12312 = PLANE ( 'NONE',  #8931 ) ;
#12313 = PRODUCT_DEFINITION_SHAPE ( 'NONE', 'NONE',  #8107 ) ;
#12314 = LINE ( 'NONE', #7301, #4371 ) ;
#12315 = PLANE ( 'NONE',  #13277 ) ;
#12316 = DIRECTION ( 'NONE',  ( 0.4330127018922209636, 0.2500000000000048850, 0.8660254037844363761 ) ) ;
#12317 = CARTESIAN_POINT ( 'NONE',  ( 218.5801281010350863, 37.63702161621608866, -16.29291827778579815 ) ) ;
#12318 = VECTOR ( 'NONE', #8004, 1000.000000000000114 ) ;
#12319 = ORIENTED_EDGE ( 'NONE', *, *, #9648, .T. ) ;
#12320 = CARTESIAN_POINT ( 'NONE',  ( 212.0325450024346026, 6.287737754125841683, -1.381056684022670344 ) ) ;
#12321 = DIRECTION ( 'NONE',  ( -0.5000000000000051070, 0.8660254037844359321, -0.000000000000000000 ) ) ;
#12322 = DIRECTION ( 'NONE',  ( 0.000000000000000000, 0.000000000000000000, -1.000000000000000000 ) ) ;
#12323 = ORIENTED_EDGE ( 'NONE', *, *, #17421, .T. ) ;
#12324 = CARTESIAN_POINT ( 'NONE',  ( 76.18374514106935180, 68.28054226513678771, 0.08292959599182991859 ) ) ;
#12325 = ORIENTED_EDGE ( 'NONE', *, *, #8214, .F. ) ;
#12326 = EDGE_LOOP ( 'NONE', ( #6622, #20757 ) ) ;
#12327 = DIRECTION ( 'NONE',  ( 0.000000000000000000, 0.8660254037844379305, -0.5000000000000014433 ) ) ;
#12328 = DIRECTION ( 'NONE',  ( 0.5000000000000054401, -0.8660254037844354880, 0.000000000000000000 ) ) ;
#12329 = CONICAL_SURFACE ( 'NONE', #6882, 13.07248899748297433, 0.6693469023067423196 ) ;
#12330 = PLANE ( 'NONE',  #7234 ) ;
#12331 = VERTEX_POINT ( 'NONE', #1710 ) ;
#12332 = DIRECTION ( 'NONE',  ( 0.000000000000000000, -1.155257860108280923E-16, 1.000000000000000000 ) ) ;
#12333 = CARTESIAN_POINT ( 'NONE',  ( 217.9607779367323985, 9.710404634561534465, -8.669480444820854004 ) ) ;
#12334 = DIRECTION ( 'NONE',  ( -0.5000000000000054401, 0.8660254037844354880, -0.000000000000000000 ) ) ;
#12335 = CARTESIAN_POINT ( 'NONE',  ( 204.3878836909736094, 13.42109587188279285, -25.81526893633800412 ) ) ;
#12336 = VERTEX_POINT ( 'NONE', #1611 ) ;
#12337 = EDGE_CURVE ( 'NONE', #8757, #3195, #4820, .T. ) ;
#12338 = DIRECTION ( 'NONE',  ( 0.000000000000000000, 0.5746640192525248603, 0.8183894335684777088 ) ) ;
#12339 = CARTESIAN_POINT ( 'NONE',  ( 184.9952905943350743, 3.535126980567765642, 0.9999999999999187317 ) ) ;
#12340 = PLANE ( 'NONE',  #10170 ) ;
#12341 = B_SPLINE_CURVE_WITH_KNOTS ( 'NONE', 3,
 ( #8135, #3273, #7729, #1688, #13039, #19478, #2870, #9306, #1282, #12624, #6134, #14852, #2002, #10028, #13244, #3583, #3792, #5367, #13138, #15168, #16523, #5265 ),
 .UNSPECIFIED., .F., .F.,
 ( 4, 2, 2, 2, 2, 2, 2, 2, 2, 2, 4 ),
 ( 0.01579861840763206043, 0.01629201531149390356, 0.01678541221535574668, 0.01777220602307943639, 0.01875899983080312264, 0.01974579363852681235, 0.02073258744625049860, 0.02122598435011234519, 0.02171938125397419178, 0.02270617506169788843, 0.02369296886942158509 ),
 .UNSPECIFIED. ) ;
#12342 = CARTESIAN_POINT ( 'NONE',  ( 77.00490953756757051, 160.5799536996104564, 56.00000000000000711 ) ) ;
#12343 = EDGE_LOOP ( 'NONE', ( #6506, #19374, #11481, #6401, #11133, #10357 ) ) ;
#12344 = FACE_OUTER_BOUND ( 'NONE', #19697, .T. ) ;
#12345 = CARTESIAN_POINT ( 'NONE',  ( 228.7571489801074449, 37.84343886304702664, -17.13000457754914052 ) ) ;
#12346 = EDGE_CURVE ( 'NONE', #3585, #12762, #1817, .T. ) ;
#12347 = CARTESIAN_POINT ( 'NONE',  ( 195.9720064151970007, 8.562186861246273040, -6.376588578941770002 ) ) ;
#12348 = CARTESIAN_POINT ( 'NONE',  ( 172.3972143829816162, 19.35563505625646030, -14.00000000000000533 ) ) ;
#12350 = ORIENTED_EDGE ( 'NONE', *, *, #12388, .F. ) ;
#12349 = EDGE_LOOP ( 'NONE', ( #6541, #16720, #15098, #465 ) ) ;
#12351 = EDGE_LOOP ( 'NONE', ( #11003, #12766, #3718, #798, #10253, #6943 ) ) ;
#12352 = DIRECTION ( 'NONE',  ( 0.000000000000000000, 0.8660254037844375974, -0.5000000000000019984 ) ) ;
#12353 = CARTESIAN_POINT ( 'NONE',  ( 5.000000000000000000, 0.000000000000000000, 0.000000000000000000 ) ) ;
#12354 = ORIENTED_EDGE ( 'NONE', *, *, #18046, .T. ) ;
#12355 = PRODUCT_DEFINITION_CONTEXT ( 'detailed design', #2851, 'design' ) ;
#12356 = DIRECTION ( 'NONE',  ( -0.5000000000000058842, 0.8660254037844351549, 0.000000000000000000 ) ) ;
#12357 = DIRECTION ( 'NONE',  ( 0.000000000000000000, -0.5000000000000009992, -0.8660254037844380415 ) ) ;
#12358 = AXIS2_PLACEMENT_3D ( 'NONE', #8414, #380, #20085 ) ;
#12359 = DIRECTION ( 'NONE',  ( -0.3155439721630312055, 0.5465381918084657453, 0.7757112907044146910 ) ) ;
#12360 = EDGE_CURVE ( 'NONE', #15276, #3499, #1791, .T. ) ;
#12361 = CARTESIAN_POINT ( 'NONE',  ( 218.5272241891094325, 10.03744253085286964, -18.09983247376310089 ) ) ;
#12362 = ORIENTED_EDGE ( 'NONE', *, *, #8734, .T. ) ;
#12363 = CARTESIAN_POINT ( 'NONE',  ( 215.0732969577928202, 15.28931427629719231, -8.544894389633146403 ) ) ;
#12364 = CARTESIAN_POINT ( 'NONE',  ( 179.0478494775924503, 57.83639716978969147, -9.087049258353273373 ) ) ;
#12365 = DIRECTION ( 'NONE',  ( -0.5000000000000054401, 0.8660254037844354880, -0.000000000000000000 ) ) ;
#12366 = ADVANCED_FACE ( 'NONE', ( #16439 ), #10057, .F. ) ;
#12367 = DIRECTION ( 'NONE',  ( -0.5000000000000061062, 1.060575238724902601E-16, -0.8660254037844351549 ) ) ;
#12368 = DIRECTION ( 'NONE',  ( 0.000000000000000000, 0.000000000000000000, -1.000000000000000000 ) ) ;
#12369 = EDGE_CURVE ( 'NONE', #3334, #513, #18035, .T. ) ;
#12371 = VERTEX_POINT ( 'NONE', #14873 ) ;
#12370 = VERTEX_POINT ( 'NONE', #13370 ) ;
#12372 = ORIENTED_EDGE ( 'NONE', *, *, #3719, .F. ) ;
#12373 = FACE_OUTER_BOUND ( 'NONE', #11521, .T. ) ;
#12374 = ORIENTED_EDGE ( 'NONE', *, *, #14090, .T. ) ;
#12375 = CIRCLE ( 'NONE', #6926, 11.98469917212512215 ) ;
#12376 = DIRECTION ( 'NONE',  ( 0.000000000000000000, -1.000000000000000000, 0.000000000000000000 ) ) ;
#12377 = CARTESIAN_POINT ( 'NONE',  ( 79.36047190431935405, 49.50000000000002842, -12.49999999998710898 ) ) ;
#12378 = LINE ( 'NONE', #7369, #7310 ) ;
#12379 = ADVANCED_FACE ( 'NONE', ( #19925, #10373 ), #16545, .T. ) ;
#12380 = CARTESIAN_POINT ( 'NONE',  ( 195.4216187824635824, 18.83910615367633667, -14.00000000000005507 ) ) ;
#12381 = B_SPLINE_CURVE_WITH_KNOTS ( 'NONE', 3,
 ( #9150, #18921, #9252, #15757 ),
 .UNSPECIFIED., .F., .F.,
 ( 4, 4 ),
 ( 4.507033345943735000E-05, 0.0007177211255159268027 ),
 .UNSPECIFIED. ) ;
#12382 = CARTESIAN_POINT ( 'NONE',  ( 193.6293134455680445, 7.209632444602317669, -12.64773574313024085 ) ) ;
#12383 = ADVANCED_BREP_SHAPE_REPRESENTATION ( '', ( #3700, #18233 ), #14867 ) ;
#12384 = ORIENTED_EDGE ( 'NONE', *, *, #20306, .T. ) ;
#12385 = VERTEX_POINT ( 'NONE', #13267 ) ;
#12386 = CONICAL_SURFACE ( 'NONE', #17797, 4.509097725792825528, 0.5235987755983015912 ) ;
#12387 = CARTESIAN_POINT ( 'NONE',  ( 221.6908239000964613, 32.21911363929024930, -13.37096421021202630 ) ) ;
#12388 = EDGE_CURVE ( 'NONE', #16780, #18827, #18680, .T. ) ;
#12389 = VECTOR ( 'NONE', #8471, 1000.000000000000114 ) ;
#12390 = LINE ( 'NONE', #17249, #3459 ) ;
#12391 = CARTESIAN_POINT ( 'NONE',  ( -21.34090909479325759, 45.27736777337857887, -11.32243216392325458 ) ) ;
#12392 = DIRECTION ( 'NONE',  ( -0.8660254037844372643, -0.5000000000000027756, 0.000000000000000000 ) ) ;
#12393 = VECTOR ( 'NONE', #11049, 1000.000000000000114 ) ;
#12394 = EDGE_CURVE ( 'NONE', #340, #18388, #644, .T. ) ;
#12395 = CARTESIAN_POINT ( 'NONE',  ( 214.8766030929655813, 15.35276292467472103, -19.36714384557541990 ) ) ;
#12396 = DIRECTION ( 'NONE',  ( 0.000000000000000000, 0.5746640192525130919, -0.8183894335684859245 ) ) ;
#12398 = VERTEX_POINT ( 'NONE', #16862 ) ;
#12397 = ORIENTED_EDGE ( 'NONE', *, *, #2373, .F. ) ;
#12399 = CARTESIAN_POINT ( 'NONE',  ( 226.8930288651464764, 41.72514874607323065, -11.06956603356934643 ) ) ;
#12400 = CARTESIAN_POINT ( 'NONE',  ( 208.4761278624580711, 5.007259451653140125, -14.00000000000005507 ) ) ;
#12401 = CARTESIAN_POINT ( 'NONE',  ( 228.5829838626408446, 38.79806082790808830, -10.60500809762013752 ) ) ;
#12402 = ORIENTED_EDGE ( 'NONE', *, *, #7150, .T. ) ;
#12403 = CARTESIAN_POINT ( 'NONE',  ( 209.3577481411912231, 3.480248335904271961, -14.00000000000005507 ) ) ;
#12404 = PLANE ( 'NONE',  #8129 ) ;
#12405 = CARTESIAN_POINT ( 'NONE',  ( -33.21445101426393620, 51.72190322358105874, -5.511193331917786153 ) ) ;
#12406 = CIRCLE ( 'NONE', #4609, 2.961423854602166283 ) ;
#12407 = LINE ( 'NONE', #5906, #3591 ) ;
#12408 = ORIENTED_EDGE ( 'NONE', *, *, #11057, .T. ) ;
#12409 = ADVANCED_FACE ( 'NONE', ( #3817 ), #20062, .T. ) ;
#12410 = ADVANCED_FACE ( 'NONE', ( #16654 ), #5186, .F. ) ;
#12411 = ORIENTED_EDGE ( 'NONE', *, *, #1923, .T. ) ;
#12412 = VECTOR ( 'NONE', #7290, 1000.000000000000114 ) ;
#12413 = LINE ( 'NONE', #15902, #13789 ) ;
#12414 = CIRCLE ( 'NONE', #16799, 3.999999999999999112 ) ;
#12415 = CARTESIAN_POINT ( 'NONE',  ( 218.7490010597510945, 37.34452507169554991, -11.35524774226742650 ) ) ;
#12416 = CARTESIAN_POINT ( 'NONE',  ( 79.17199999999999704, 3.469446951953613573E-17, 5.000000000000035527 ) ) ;
#12417 = CARTESIAN_POINT ( 'NONE',  ( 229.1914409901575880, 36.76471627775831763, -11.94979443502199956 ) ) ;
#12418 = EDGE_CURVE ( 'NONE', #16451, #13417, #6888, .T. ) ;
#12419 = CARTESIAN_POINT ( 'NONE',  ( 227.9553588074475670, 39.88513931160575510, -14.00000000000005507 ) ) ;
#12420 = CARTESIAN_POINT ( 'NONE',  ( -31.74999999999995737, 0.000000000000000000, 8.000000000000000000 ) ) ;
#12421 = CARTESIAN_POINT ( 'NONE',  ( 226.8410035935495728, 41.81525915975633012, -17.20332536629370068 ) ) ;
#12422 = TOROIDAL_SURFACE ( 'NONE', #5952, 1.003313105759043200, 1.000000000000000000 ) ;
#12423 = DIRECTION ( 'NONE',  ( -0.8660254037844355990, -0.5000000000000054401, -1.682612938603036717E-14 ) ) ;
#12424 = FACE_BOUND ( 'NONE', #15647, .T. ) ;
#12425 = DIRECTION ( 'NONE',  ( 0.8660254037844370423, 0.5000000000000026645, -0.000000000000000000 ) ) ;
#12426 = CONICAL_SURFACE ( 'NONE', #3266, 13.07248899748297433, 0.6693469023067423196 ) ;
#12427 = VERTEX_POINT ( 'NONE', #7099 ) ;
#12428 = AXIS2_PLACEMENT_3D ( 'NONE', #9058, #13644, #12368 ) ;
#12429 = EDGE_CURVE ( 'NONE', #13646, #5066, #5287, .T. ) ;
#12430 = CARTESIAN_POINT ( 'NONE',  ( 81.96650144582014264, 64.62052529102815868, 0.4991931981429228449 ) ) ;
#12431 = B_SPLINE_CURVE_WITH_KNOTS ( 'NONE', 3,
 ( #8094, #3343, #14713, #165 ),
 .UNSPECIFIED., .F., .F.,
 ( 4, 4 ),
 ( 5.847970038296026269E-07, 0.0005665110192997313120 ),
 .UNSPECIFIED. ) ;
#12432 = ORIENTED_EDGE ( 'NONE', *, *, #5879, .F. ) ;
#12433 = EDGE_LOOP ( 'NONE', ( #12307, #5753, #152, #16475 ) ) ;
#12434 = CARTESIAN_POINT ( 'NONE',  ( -4.015193415984987801, 74.73312780907788522, 3.553696893467043871 ) ) ;
#12435 = APPLICATION_PROTOCOL_DEFINITION ( 'draft international standard', 'automotive_design', 1998, #15314 ) ;
#12436 = CARTESIAN_POINT ( 'NONE',  ( 210.0179110316588265, 27.28626740294374287, -14.01558723443205068 ) ) ;
#12437 = ORIENTED_EDGE ( 'NONE', *, *, #14894, .F. ) ;
#12438 = AXIS2_PLACEMENT_3D ( 'NONE', #1962, #16698, #484 ) ;
#12439 = FILL_AREA_STYLE_COLOUR ( '', #12136 ) ;
#12440 = CARTESIAN_POINT ( 'NONE',  ( 226.8930288651464764, 41.72514874607323065, -11.06956603356934643 ) ) ;
#12441 = PLANE ( 'NONE',  #11393 ) ;
#12442 = CARTESIAN_POINT ( 'NONE',  ( 34.99529059433364608, 263.3427481158985302, 1.000000000000017097 ) ) ;
#12443 = DIRECTION ( 'NONE',  ( 0.5000000000000044409, -0.8660254037844360431, -0.000000000000000000 ) ) ;
#12444 = CARTESIAN_POINT ( 'NONE',  ( 216.3683575532813848, 33.19538101841231992, -14.00000000000004441 ) ) ;
#12445 = CARTESIAN_POINT ( 'NONE',  ( 199.4075733045063146, 6.421714412205289157, -4.379064819896086647 ) ) ;
#12446 = FACE_OUTER_BOUND ( 'NONE', #10842, .T. ) ;
#12447 = ORIENTED_EDGE ( 'NONE', *, *, #19854, .F. ) ;
#12448 = LINE ( 'NONE', #2898, #3056 ) ;
#12449 = CARTESIAN_POINT ( 'NONE',  ( -4.442041072745785080, 70.83821676753269969, 4.766221741044108562 ) ) ;
#12450 = CIRCLE ( 'NONE', #2968, 3.619616396367202782 ) ;
#12451 = DIRECTION ( 'NONE',  ( 0.6634139481689351747, 0.3830222215594923374, -0.6427876096865405842 ) ) ;
#12452 = CARTESIAN_POINT ( 'NONE',  ( 182.3972143829817867, 2.035126980567750099, -6.000000000000071942 ) ) ;
#12453 = AXIS2_PLACEMENT_3D ( 'NONE', #9362, #17659, #6386 ) ;
#12455 = EDGE_LOOP ( 'NONE', ( #15543, #14516, #18443, #607 ) ) ;
#12454 = VERTEX_POINT ( 'NONE', #2137 ) ;
#12456 = PLANE ( 'NONE',  #6129 ) ;
#12457 = LINE ( 'NONE', #7244, #10867 ) ;
#12458 = ORIENTED_EDGE ( 'NONE', *, *, #8464, .F. ) ;
#12459 = CARTESIAN_POINT ( 'NONE',  ( 205.5965122587965084, 9.994899983462953941, -14.00000000000005507 ) ) ;
#12460 = CARTESIAN_POINT ( 'NONE',  ( 37.00490953756720813, 229.8619860023653132, 26.00000000000001776 ) ) ;
#12461 = ORIENTED_EDGE ( 'NONE', *, *, #18053, .T. ) ;
#12462 = EDGE_CURVE ( 'NONE', #20638, #15824, #1442, .T. ) ;
#12463 = CARTESIAN_POINT ( 'NONE',  ( 229.2052127624425850, 36.74086286845060556, -16.00491213559321579 ) ) ;
#12464 = AXIS2_PLACEMENT_3D ( 'NONE', #20378, #5531, #5631 ) ;
#12465 = ORIENTED_EDGE ( 'NONE', *, *, #1330, .T. ) ;
#12466 = CARTESIAN_POINT ( 'NONE',  ( 34.99529059433362477, 263.3427481158986438, 1.000000000000017097 ) ) ;
#12467 = DIRECTION ( 'NONE',  ( -0.5000000000000025535, 0.8660254037844372643, 0.000000000000000000 ) ) ;
#12468 = CARTESIAN_POINT ( 'NONE',  ( 0.000000000000000000, 2.342598717236899830, -4.057500000000030305 ) ) ;
#12469 = FACE_OUTER_BOUND ( 'NONE', #16330, .T. ) ;
#12470 = CARTESIAN_POINT ( 'NONE',  ( 214.9383172013976093, 8.738206206044257129, -4.003039906354144861 ) ) ;
#12471 = ORIENTED_EDGE ( 'NONE', *, *, #15754, .T. ) ;
#12472 = VERTEX_POINT ( 'NONE', #13161 ) ;
#12473 = CARTESIAN_POINT ( 'NONE',  ( 48.39721438298045797, 234.1299351947966443, -13.99999999999998046 ) ) ;
#12474 = ORIENTED_EDGE ( 'NONE', *, *, #8504, .T. ) ;
#12475 = VERTEX_POINT ( 'NONE', #14771 ) ;
#12476 = VECTOR ( 'NONE', #13992, 1000.000000000000000 ) ;
#12477 = CARTESIAN_POINT ( 'NONE',  ( -18.23302563531977327, 10.61358200216139203, 12.30279443686337082 ) ) ;
#12478 = PRODUCT_DEFINITION_SHAPE ( 'NONE', 'NONE',  #20952 ) ;
#12479 = DIRECTION ( 'NONE',  ( 0.5000000000000041078, -0.8660254037844363761, 0.000000000000000000 ) ) ;
#12480 = LINE ( 'NONE', #19147, #14128 ) ;
#12481 = DIRECTION ( 'NONE',  ( 0.000000000000000000, 0.000000000000000000, -1.000000000000000000 ) ) ;
#12482 = DIRECTION ( 'NONE',  ( -0.000000000000000000, -1.000000000000000000, 0.000000000000000000 ) ) ;
#12483 = EDGE_CURVE ( 'NONE', #13646, #6959, #12963, .T. ) ;
#12484 = ORIENTED_EDGE ( 'NONE', *, *, #16398, .T. ) ;
#12485 = ADVANCED_FACE ( 'NONE', ( #9947 ), #13588, .F. ) ;
#12486 = CARTESIAN_POINT ( 'NONE',  ( 205.5965122587965084, 9.994899983462953941, -14.00000000000005507 ) ) ;
#12487 = CARTESIAN_POINT ( 'NONE',  ( 87.00490953756771262, 143.2594456239216925, 21.00000000000000711 ) ) ;
#12488 = CARTESIAN_POINT ( 'NONE',  ( -22.50947703420033008, 49.61991195516749542, -10.68093576282688240 ) ) ;
#12489 = FACE_OUTER_BOUND ( 'NONE', #11029, .T. ) ;
#12490 = CARTESIAN_POINT ( 'NONE',  ( 228.0992539300394810, 39.63590564831545748, -18.24372585368656630 ) ) ;
#12491 = PLANE ( 'NONE',  #548 ) ;
#12493 = ORIENTED_EDGE ( 'NONE', *, *, #561, .T. ) ;
#12492 = EDGE_LOOP ( 'NONE', ( #2672, #7528, #15241, #8012, #12760 ) ) ;
#12494 = DIRECTION ( 'NONE',  ( -1.000000000000000000, -0.000000000000000000, -0.000000000000000000 ) ) ;
#12495 = LINE ( 'NONE', #15693, #12899 ) ;
#12496 = CARTESIAN_POINT ( 'NONE',  ( -3.580465574138951723, 80.00000000005285017, -1.424835221694952025 ) ) ;
#12497 = ORIENTED_EDGE ( 'NONE', *, *, #11420, .T. ) ;
#12498 = ORIENTED_EDGE ( 'NONE', *, *, #9794, .F. ) ;
#12499 = LINE ( 'NONE', #18959, #4471 ) ;
#12500 = CARTESIAN_POINT ( 'NONE',  ( 199.2243387870319395, 21.03182819120163671, -14.00000000000005507 ) ) ;
#12501 = CARTESIAN_POINT ( 'NONE',  ( -33.51494856915631715, 53.43435578398468522, -2.915686290500575151 ) ) ;
#12502 = CARTESIAN_POINT ( 'NONE',  ( -26.77504448057880637, 9.902224835466700625, 6.371987388190586188 ) ) ;
#12503 = ORIENTED_EDGE ( 'NONE', *, *, #4956, .F. ) ;
#12504 = EDGE_CURVE ( 'NONE', #140, #12601, #20039, .T. ) ;
#12505 = VECTOR ( 'NONE', #13892, 1000.000000000000227 ) ;
#12506 = VERTEX_POINT ( 'NONE', #226 ) ;
#12507 = DIRECTION ( 'NONE',  ( -0.5000000000000054401, 0.8660254037844354880, -0.000000000000000000 ) ) ;
#12508 = ORIENTED_EDGE ( 'NONE', *, *, #11329, .F. ) ;
#12509 = ADVANCED_FACE ( 'NONE', ( #6666 ), #19605, .F. ) ;
#12510 = LINE ( 'NONE', #17490, #14040 ) ;
#12511 = CARTESIAN_POINT ( 'NONE',  ( 28.00000000000001066, 64.25000000000000000, 75.00000000000000000 ) ) ;
#12512 = CARTESIAN_POINT ( 'NONE',  ( 81.11443760607866693, 65.90576556446161760, -25.47662540745488613 ) ) ;
#12513 = EDGE_CURVE ( 'NONE', #20505, #7315, #2451, .T. ) ;
#12514 = ORIENTED_EDGE ( 'NONE', *, *, #12140, .F. ) ;
#12515 = CARTESIAN_POINT ( 'NONE',  ( 195.0945143319839872, 3.400519391596340757, -15.43274561385865695 ) ) ;
#12516 = CARTESIAN_POINT ( 'NONE',  ( -28.45531017328980994, 78.99734867018936768, 1.332611642696158505 ) ) ;
#12517 = DIRECTION ( 'NONE',  ( 0.000000000000000000, 6.938893903907177533E-18, 1.000000000000000000 ) ) ;
#12518 = EDGE_CURVE ( 'NONE', #18037, #15665, #13615, .T. ) ;
#12519 = FACE_OUTER_BOUND ( 'NONE', #11185, .T. ) ;
#12520 = LINE ( 'NONE', #7409, #4866 ) ;
#12521 = CARTESIAN_POINT ( 'NONE',  ( -31.74999999999995737, 0.000000000000000000, 0.000000000000000000 ) ) ;
#12522 = EDGE_CURVE ( 'NONE', #10554, #6749, #13982, .T. ) ;
#12523 = VECTOR ( 'NONE', #5030, 1000.000000000000000 ) ;
#12524 = ORIENTED_EDGE ( 'NONE', *, *, #19194, .T. ) ;
#12525 = CARTESIAN_POINT ( 'NONE',  ( 79.68127019285799406, 68.50330513000922394, 0.4783565974505511464 ) ) ;
#12526 = ORIENTED_EDGE ( 'NONE', *, *, #2414, .T. ) ;
#12527 = ORIENTED_EDGE ( 'NONE', *, *, #6267, .F. ) ;
#12528 = CARTESIAN_POINT ( 'NONE',  ( -3.057294037196384817, 74.04855861174505094, -0.5148205403777549316 ) ) ;
#12529 = DIRECTION ( 'NONE',  ( 0.3886714912512297393, 0.2243995901002339699, 0.8936326403234117199 ) ) ;
#12530 = ADVANCED_FACE ( 'NONE', ( #961 ), #7305, .T. ) ;
#12531 = LINE ( 'NONE', #12217, #1156 ) ;
#12532 = ORIENTED_EDGE ( 'NONE', *, *, #8472, .T. ) ;
#12533 = CARTESIAN_POINT ( 'NONE',  ( 202.0355941508142337, 1.288815579510670828, -24.01557619556968248 ) ) ;
#12534 = ADVANCED_FACE ( 'NONE', ( #20555 ), #15600, .T. ) ;
#12535 = AXIS2_PLACEMENT_3D ( 'NONE', #9577, #16075, #4913 ) ;
#12536 = EDGE_CURVE ( 'NONE', #12038, #20059, #4247, .T. ) ;
#12537 = LINE ( 'NONE', #4265, #9424 ) ;
#12538 = DIRECTION ( 'NONE',  ( -0.5000000000000049960, 0.8660254037844358210, -0.000000000000000000 ) ) ;
#12539 = LINE ( 'NONE', #17305, #15632 ) ;
#12540 = VECTOR ( 'NONE', #17253, 1000.000000000000114 ) ;
#12541 = CARTESIAN_POINT ( 'NONE',  ( 63.47128125378750951, 81.72905832825074413, -20.14264400969036828 ) ) ;
#12542 = DIRECTION ( 'NONE',  ( -0.8660254037844378194, -0.5000000000000013323, -0.000000000000000000 ) ) ;
#12543 = EDGE_CURVE ( 'NONE', #38, #2596, #11264, .T. ) ;
#12544 = CARTESIAN_POINT ( 'NONE',  ( 85.37797649651368204, 230.0773763115391262, -0.9999999999999826805 ) ) ;
#12545 = FACE_OUTER_BOUND ( 'NONE', #13513, .T. ) ;
#12546 = CARTESIAN_POINT ( 'NONE',  ( -15.99999999999999289, 20.09941697557067997, 4.999999999999989342 ) ) ;
#12547 = VERTEX_POINT ( 'NONE', #5706 ) ;
#12548 = CARTESIAN_POINT ( 'NONE',  ( 217.1683686445515207, 38.56875433448770707, -13.99751724578378997 ) ) ;
#12549 = DIRECTION ( 'NONE',  ( 0.000000000000000000, 0.000000000000000000, -1.000000000000000000 ) ) ;
#12550 = EDGE_CURVE ( 'NONE', #10440, #7006, #8209, .T. ) ;
#12551 = DIRECTION ( 'NONE',  ( -0.8660254037844355990, -0.5000000000000055511, 0.000000000000000000 ) ) ;
#12552 = CARTESIAN_POINT ( 'NONE',  ( 227.3801919349025411, 40.88135755768454516, -17.38313153181858439 ) ) ;
#12553 = CONICAL_SURFACE ( 'NONE', #4415, 4.509097725792825528, 0.5235987755983015912 ) ;
#12554 = DIRECTION ( 'NONE',  ( -1.000000000000000000, 0.000000000000000000, 1.218100516808353647E-16 ) ) ;
#12555 = EDGE_CURVE ( 'NONE', #12398, #13274, #18052, .T. ) ;
#12557 = ORIENTED_EDGE ( 'NONE', *, *, #9539, .F. ) ;
#12556 = ORIENTED_EDGE ( 'NONE', *, *, #1881, .T. ) ;
#12558 = AXIS2_PLACEMENT_3D ( 'NONE', #20610, #4612, #12683 ) ;
#12559 = EDGE_LOOP ( 'NONE', ( #16012, #12581, #5610, #9290 ) ) ;
#12560 = DIRECTION ( 'NONE',  ( 0.000000000000000000, -0.4999999999999985012, 0.8660254037844394848 ) ) ;
#12561 = LINE ( 'NONE', #7664, #10198 ) ;
#12562 = VERTEX_POINT ( 'NONE', #6028 ) ;
#12563 = PRODUCT_DEFINITION_CONTEXT ( 'detailed design', #5921, 'design' ) ;
#12564 = CARTESIAN_POINT ( 'NONE',  ( 226.2863802629166230, 42.77589494747574861, -12.60011953066305246 ) ) ;
#12565 = DIRECTION ( 'NONE',  ( 0.7366891686653773696, 0.000000000000000000, -0.6762315200958287642 ) ) ;
#12566 = ADVANCED_FACE ( 'NONE', ( #13896 ), #17390, .T. ) ;
#12567 = FACE_OUTER_BOUND ( 'NONE', #17137, .T. ) ;
#12568 = CONICAL_SURFACE ( 'NONE', #15961, 3.078786038154920579, 0.8168758188741392923 ) ;
#12569 = DIRECTION ( 'NONE',  ( -0.000000000000000000, -1.000000000000000000, -0.000000000000000000 ) ) ;
#12570 =( NAMED_UNIT ( * ) PLANE_ANGLE_UNIT ( ) SI_UNIT ( $, .RADIAN. ) );
#12571 = CIRCLE ( 'NONE', #16967, 5.000000000000005329 ) ;
#12572 = ORIENTED_EDGE ( 'NONE', *, *, #3830, .F. ) ;
#12573 = CARTESIAN_POINT ( 'NONE',  ( 228.1017308963825201, 39.63161541676044664, -10.39224118001587982 ) ) ;
#12574 = CARTESIAN_POINT ( 'NONE',  ( 225.7886100484356575, 42.98509911694870311, -14.55116774095995424 ) ) ;
#12575 = LINE ( 'NONE', #4710, #11851 ) ;
#12576 = PLANE ( 'NONE',  #7114 ) ;
#12577 = ORIENTED_EDGE ( 'NONE', *, *, #11499, .F. ) ;
#12578 = DIRECTION ( 'NONE',  ( -0.4814586436739051178, 0.8339108325863908711, -0.2697967711570247729 ) ) ;
#12579 = AXIS2_PLACEMENT_3D ( 'NONE', #9889, #11713, #13627 ) ;
#12580 = ORIENTED_EDGE ( 'NONE', *, *, #18370, .T. ) ;
#12581 = ORIENTED_EDGE ( 'NONE', *, *, #14048, .T. ) ;
#12582 = EDGE_CURVE ( 'NONE', #3560, #3499, #15713, .T. ) ;
#12583 = CARTESIAN_POINT ( 'NONE',  ( -16.33019277271582226, 10.09941697557068707, 12.50000000000000178 ) ) ;
#12584 = LINE ( 'NONE', #17354, #13256 ) ;
#12585 = DIRECTION ( 'NONE',  ( 0.5000000000000054401, -0.8660254037844354880, 0.000000000000000000 ) ) ;
#12586 = DIRECTION ( 'NONE',  ( 0.4084849465052217132, -0.7075166814740940779, 0.5766803221148711911 ) ) ;
#12587 = SURFACE_SIDE_STYLE ('',( #15571 ) ) ;
#12588 = AXIS2_PLACEMENT_3D ( 'NONE', #9154, #4510, #14060 ) ;
#12589 = VERTEX_POINT ( 'NONE', #5603 ) ;
#12590 = CARTESIAN_POINT ( 'NONE',  ( 219.8041001712509512, 35.51703980355691215, -10.43865930680574827 ) ) ;
#12591 = EDGE_CURVE ( 'NONE', #504, #884, #7539, .T. ) ;
#12592 = MECHANICAL_DESIGN_GEOMETRIC_PRESENTATION_REPRESENTATION (  '', ( #6820 ), #15663 ) ;
#12593 = CARTESIAN_POINT ( 'NONE',  ( 213.9717500725588479, 7.407338323375970646, -24.35247136794745515 ) ) ;
#12594 = CARTESIAN_POINT ( 'NONE',  ( -8.885764546551122578, 45.08372817709340552, -10.30101951839246333 ) ) ;
#12595 = CARTESIAN_POINT ( 'NONE',  ( 199.2231352798572743, 21.03391272677540513, -14.00000000000005507 ) ) ;
#12596 = AXIS2_PLACEMENT_3D ( 'NONE', #18041, #14878, #14464 ) ;
#12597 = CONICAL_SURFACE ( 'NONE', #8510, 4.509097725792825528, 0.5235987755983015912 ) ;
#12598 = DIRECTION ( 'NONE',  ( 0.4711304610594118647, -0.8160218955482464454, 0.3348796121709901596 ) ) ;
#12599 = CARTESIAN_POINT ( 'NONE',  ( 190.1809276776941715, 15.83337972362198265, -20.84195174293567376 ) ) ;
#12600 = ORIENTED_EDGE ( 'NONE', *, *, #61, .T. ) ;
#12601 = VERTEX_POINT ( 'NONE', #12199 ) ;
#12602 = CARTESIAN_POINT ( 'NONE',  ( 195.3173534746875930, 3.529175630622251258, -16.89203719259486647 ) ) ;
#12603 = DIRECTION ( 'NONE',  ( -0.4988343845952723510, 0.8640064986813598136, 0.06824241336466070618 ) ) ;
#12604 = AXIS2_PLACEMENT_3D ( 'NONE', #8289, #4910, #9676 ) ;
#12605 = CARTESIAN_POINT ( 'NONE',  ( -3.645413219200714039, 80.00000000007608492, -1.908121642414585484 ) ) ;
#12606 = ORIENTED_EDGE ( 'NONE', *, *, #15085, .F. ) ;
#12607 = VERTEX_POINT ( 'NONE', #4141 ) ;
#12608 = EDGE_CURVE ( 'NONE', #2250, #12799, #10596, .T. ) ;
#12609 = CARTESIAN_POINT ( 'NONE',  ( 216.7494463307476451, 9.526248244645403318, -6.098918798390618790 ) ) ;
#12610 = CARTESIAN_POINT ( 'NONE',  ( 195.1593178475889374, 3.614956399211269655, -15.42323214253203112 ) ) ;
#12611 = CARTESIAN_POINT ( 'NONE',  ( -16.80570248528584543, 50.47613221401184802, -16.24930194057697364 ) ) ;
#12612 = CARTESIAN_POINT ( 'NONE',  ( -27.37786364650417070, 9.617207265011291639, -5.186836524664776071 ) ) ;
#12613 = VERTEX_POINT ( 'NONE', #12317 ) ;
#12614 = ADVANCED_FACE ( 'NONE', ( #2663 ), #20142, .F. ) ;
#12615 = ORIENTED_EDGE ( 'NONE', *, *, #17670, .T. ) ;
#12616 = DIRECTION ( 'NONE',  ( 0.000000000000000000, -0.5000000000000009992, -0.8660254037844380415 ) ) ;
#12617 = CARTESIAN_POINT ( 'NONE',  ( 1.500000000000001332, 0.000000000000000000, 8.000000000000000000 ) ) ;
#12618 = LINE ( 'NONE', #16282, #6554 ) ;
#12619 = DIRECTION ( 'NONE',  ( 0.8660254037844372643, 0.5000000000000027756, -0.000000000000000000 ) ) ;
#12620 = DIRECTION ( 'NONE',  ( 0.5000000000000046629, -0.8660254037844359321, 0.000000000000000000 ) ) ;
#12621 = CIRCLE ( 'NONE', #16242, 5.000000000000005329 ) ;
#12622 = CARTESIAN_POINT ( 'NONE',  ( 225.9571642014708743, 43.01964481660166228, -13.96059298729438503 ) ) ;
#12623 = CARTESIAN_POINT ( 'NONE',  ( -27.89556006008164246, 56.02656468610143037, 3.843087363396194611 ) ) ;
#12624 = CARTESIAN_POINT ( 'NONE',  ( -19.97143893519406888, 18.15431163985882890, 11.85386933495461825 ) ) ;
#12625 = EDGE_LOOP ( 'NONE', ( #20594, #11240, #10902 ) ) ;
#12626 = CARTESIAN_POINT ( 'NONE',  ( 63.15554463217812042, 234.5677573683057062, -14.00000000000003020 ) ) ;
#12627 = DIRECTION ( 'NONE',  ( -1.000000000000000000, 0.000000000000000000, 0.000000000000000000 ) ) ;
#12628 = CARTESIAN_POINT ( 'NONE',  ( 226.3610044743459184, 41.99368288930288884, -16.76050993469849715 ) ) ;
#12629 = ORIENTED_EDGE ( 'NONE', *, *, #19483, .F. ) ;
#12630 = VECTOR ( 'NONE', #6160, 1000.000000000000114 ) ;
#12631 = CARTESIAN_POINT ( 'NONE',  ( 82.32960224396195770, 63.12647830926369608, 0.3677484777158103735 ) ) ;
#12632 = EDGE_CURVE ( 'NONE', #15199, #10247, #18978, .T. ) ;
#12633 = VECTOR ( 'NONE', #4728, 1000.000000000000114 ) ;
#12634 = VERTEX_POINT ( 'NONE', #7206 ) ;
#12635 = EDGE_CURVE ( 'NONE', #14752, #19313, #8252, .T. ) ;
#12636 = VERTEX_POINT ( 'NONE', #13691 ) ;
#12637 = CARTESIAN_POINT ( 'NONE',  ( -3.633681703949028119, 78.08772077735648054, 1.916778294983234154 ) ) ;
#12638 = CARTESIAN_POINT ( 'NONE',  ( 188.9132435853528591, 28.89116896218935082, -14.00000000000004086 ) ) ;
#12639 = CARTESIAN_POINT ( 'NONE',  ( -16.47102837334524850, 80.00000000000002842, -12.49810385314669148 ) ) ;
#12640 = ORIENTED_EDGE ( 'NONE', *, *, #13104, .T. ) ;
#12641 = CARTESIAN_POINT ( 'NONE',  ( 219.4100706228406921, 36.16949419502193308, -10.59705062504279915 ) ) ;
#12642 = EDGE_CURVE ( 'NONE', #11172, #18411, #4657, .T. ) ;
#12643 = ORIENTED_EDGE ( 'NONE', *, *, #3186, .F. ) ;
#12644 = CARTESIAN_POINT ( 'NONE',  ( 27.00000000000002487, 64.25000000000000000, 2.481238266578627449 ) ) ;
#12645 = ADVANCED_BREP_SHAPE_REPRESENTATION ( '', ( #3811, #18233 ), #7378 ) ;
#12646 = CARTESIAN_POINT ( 'NONE',  ( 210.7370931664818272, 12.96281575430614552, -3.762296834228894493 ) ) ;
#12647 = CARTESIAN_POINT ( 'NONE',  ( 226.4210616241540208, 42.54261998698029146, -12.08027307405517448 ) ) ;
#12648 = CARTESIAN_POINT ( 'NONE',  ( 0.2286262486868663735, 60.41611051155134504, 1.787729794976060660 ) ) ;
#12649 = DIRECTION ( 'NONE',  ( -1.000000000000000000, 0.000000000000000000, 0.000000000000000000 ) ) ;
#12650 = DIRECTION ( 'NONE',  ( -0.5000000000000008882, 0.8660254037844381525, 0.000000000000000000 ) ) ;
#12651 = EDGE_CURVE ( 'NONE', #17792, #4687, #9521, .T. ) ;
#12652 = CARTESIAN_POINT ( 'NONE',  ( 218.2721305058478265, 38.37640730049447768, -12.96641767022714120 ) ) ;
#12653 = CARTESIAN_POINT ( 'NONE',  ( 217.5085967919815175, 37.97946189697392327, -13.95097276009430587 ) ) ;
#12654 = FACE_OUTER_BOUND ( 'NONE', #15335, .T. ) ;
#12655 = ORIENTED_EDGE ( 'NONE', *, *, #1732, .T. ) ;
#12656 = CYLINDRICAL_SURFACE ( 'NONE', #3720, 13.99999999999999822 ) ;
#12657 = ADVANCED_FACE ( 'NONE', ( #19085 ), #16214, .F. ) ;
#12658 = LINE ( 'NONE', #15639, #4433 ) ;
#12659 = CARTESIAN_POINT ( 'NONE',  ( -20.99999999999998224, 15.09941697557068530, 15.00000000000000000 ) ) ;
#12660 = LINE ( 'NONE', #19019, #4472 ) ;
#12661 = VECTOR ( 'NONE', #10367, 1000.000000000000114 ) ;
#12662 = CARTESIAN_POINT ( 'NONE',  ( -28.50352467013047431, 79.99999999992598987, -0.04629550956175955412 ) ) ;
#12663 = CIRCLE ( 'NONE', #18737, 6.500000000000047962 ) ;
#12665 = ORIENTED_EDGE ( 'NONE', *, *, #20161, .F. ) ;
#12664 = VERTEX_POINT ( 'NONE', #17495 ) ;
#12666 = SURFACE_STYLE_FILL_AREA ( #12244 ) ;
#12667 = EDGE_CURVE ( 'NONE', #9307, #20827, #4961, .T. ) ;
#12668 = CARTESIAN_POINT ( 'NONE',  ( 219.8080624143775594, 36.12802536649407870, -17.81526153211078878 ) ) ;
#12669 = ADVANCED_FACE ( 'NONE', ( #6233 ), #7874, .T. ) ;
#12670 = CARTESIAN_POINT ( 'NONE',  ( 217.9776690748798558, 9.720156737717866591, -19.29168348739315775 ) ) ;
#12671 = B_SPLINE_CURVE_WITH_KNOTS ( 'NONE', 3,
 ( #450, #939, #2536, #1934, #13376, #19722, #7384, #837, #20328, #5294, #19827, #4009, #5193, #8981, #15384, #8380, #10575, #11680, #18143, #5799, #9954, #15583, #339, #8884, #8486, #16945, #10458, #6895 ),
 .UNSPECIFIED., .F., .F.,
 ( 4, 2, 2, 2, 2, 2, 2, 2, 2, 2, 2, 2, 2, 4 ),
 ( 3.469446951953614189E-18, 0.0002948126770087786098, 0.0005896253540175537501, 0.0008844380310263289446, 0.001179250708035104031, 0.001768876062052661575, 0.002358501416070219337, 0.002653314093078998435, 0.002948126770087776665, 0.003537752124105387769, 0.003832564801114191587, 0.004127377478122994971, 0.004422190155131798354, 0.004717002832140601738 ),
 .UNSPECIFIED. ) ;
#12672 = DIRECTION ( 'NONE',  ( 0.3155439721630258765, -0.5465381918084566415, 0.7757112907044233507 ) ) ;
#12673 = ORIENTED_EDGE ( 'NONE', *, *, #20015, .T. ) ;
#12674 = DIRECTION ( 'NONE',  ( 0.5000000000000007772, -0.8660254037844381525, 0.000000000000000000 ) ) ;
#12675 = VECTOR ( 'NONE', #6928, 1000.000000000000114 ) ;
#12676 = AXIS2_PLACEMENT_3D ( 'NONE', #6891, #333, #11782 ) ;
#12677 = ADVANCED_FACE ( 'NONE', ( #20860 ), #9416, .F. ) ;
#12678 =( NAMED_UNIT ( * ) SI_UNIT ( $, .STERADIAN. ) SOLID_ANGLE_UNIT ( ) );
#12679 = ORIENTED_EDGE ( 'NONE', *, *, #17191, .F. ) ;
#12680 = DIRECTION ( 'NONE',  ( -0.8660254037844355990, -0.5000000000000055511, 0.000000000000000000 ) ) ;
#12681 = CARTESIAN_POINT ( 'NONE',  ( -14.99999999999999645, 0.000000000000000000, -28.99999999999999645 ) ) ;
#12682 = DIRECTION ( 'NONE',  ( -0.8660254037844371533, -0.5000000000000027756, 0.000000000000000000 ) ) ;
#12683 = DIRECTION ( 'NONE',  ( 0.000000000000000000, 0.000000000000000000, 1.000000000000000000 ) ) ;
#12684 = ORIENTED_EDGE ( 'NONE', *, *, #8727, .T. ) ;
#12685 = DIRECTION ( 'NONE',  ( 0.000000000000000000, 0.000000000000000000, -1.000000000000000000 ) ) ;
#12686 = EDGE_CURVE ( 'NONE', #2714, #5808, #13346, .T. ) ;
#12687 = B_SPLINE_CURVE_WITH_KNOTS ( 'NONE', 3,
 ( #11861, #18325, #3897, #7379 ),
 .UNSPECIFIED., .F., .F.,
 ( 4, 4 ),
 ( 4.934226812140153520E-05, 0.0005856888230752346032 ),
 .UNSPECIFIED. ) ;
#12688 = ORIENTED_EDGE ( 'NONE', *, *, #3256, .T. ) ;
#12689 = CARTESIAN_POINT ( 'NONE',  ( -19.97299960082356307, 12.04641549374639276, 11.85335538211749018 ) ) ;
#12690 = LINE ( 'NONE', #4620, #1410 ) ;
#12691 = CARTESIAN_POINT ( 'NONE',  ( 228.7675624436089095, 38.47836134768217420, -10.76535568099436446 ) ) ;
#12692 = AXIS2_PLACEMENT_3D ( 'NONE', #14815, #18079, #13004 ) ;
#12693 = PLANE ( 'NONE',  #2921 ) ;
#12694 = DIRECTION ( 'NONE',  ( -1.000000000000000000, -0.000000000000000000, -0.000000000000000000 ) ) ;
#12695 = ORIENTED_EDGE ( 'NONE', *, *, #5232, .T. ) ;
#12696 = DIRECTION ( 'NONE',  ( 0.5000000000000051070, -0.8660254037844359321, 0.000000000000000000 ) ) ;
#12697 = DIRECTION ( 'NONE',  ( -0.5000000000000049960, 0.8660254037844357100, -0.000000000000000000 ) ) ;
#12698 = CARTESIAN_POINT ( 'NONE',  ( -7.715557909791129987, 49.87593469365641141, -9.365636588568600374 ) ) ;
#12699 = LINE ( 'NONE', #9698, #803 ) ;
#12700 = AXIS2_PLACEMENT_3D ( 'NONE', #10966, #11069, #14275 ) ;
#12701 = CARTESIAN_POINT ( 'NONE',  ( 61.99529059433385925, 216.5773763115390125, -5.999999999999973355 ) ) ;
#12702 = CARTESIAN_POINT ( 'NONE',  ( 97.64153595007269359, 199.2434332111931212, 12.98669150848017573 ) ) ;
#12703 = EDGE_LOOP ( 'NONE', ( #9195, #13238, #10350, #13200 ) ) ;
#12704 = CARTESIAN_POINT ( 'NONE',  ( 220.0163777105207714, 35.56123462361016152, -17.78601433598970161 ) ) ;
#12705 = DIRECTION ( 'NONE',  ( -0.8660254037844357100, -0.5000000000000051070, 0.000000000000000000 ) ) ;
#12706 = DIRECTION ( 'NONE',  ( -1.000000000000000000, -0.000000000000000000, -0.000000000000000000 ) ) ;
#12707 = VERTEX_POINT ( 'NONE', #12831 ) ;
#12708 = ORIENTED_EDGE ( 'NONE', *, *, #435, .F. ) ;
#12709 = VERTEX_POINT ( 'NONE', #11335 ) ;
#12710 = DIRECTION ( 'NONE',  ( -0.000000000000000000, 1.000000000000000000, -0.000000000000000000 ) ) ;
#12711 = CARTESIAN_POINT ( 'NONE',  ( 82.49529059433407951, 181.0703347563770365, 16.00000000000001066 ) ) ;
#12712 = LINE ( 'NONE', #18307, #17976 ) ;
#12713 = CARTESIAN_POINT ( 'NONE',  ( -28.38583607363177208, 8.722028531692911812, -1.718349999867211597 ) ) ;
#12714 = ORIENTED_EDGE ( 'NONE', *, *, #4468, .F. ) ;
#12715 = ORIENTED_EDGE ( 'NONE', *, *, #857, .T. ) ;
#12716 = CARTESIAN_POINT ( 'NONE',  ( 5.000000000000000000, 4.685197434473812983, -6.938893903907228378E-15 ) ) ;
#12717 = AXIS2_PLACEMENT_3D ( 'NONE', #5833, #4037, #17092 ) ;
#12718 = FACE_OUTER_BOUND ( 'NONE', #3573, .T. ) ;
#12719 = EDGE_CURVE ( 'NONE', #4703, #681, #19287, .T. ) ;
#12720 = CYLINDRICAL_SURFACE ( 'NONE', #5127, 7.960520131757808038 ) ;
#12721 = CARTESIAN_POINT ( 'NONE',  ( -27.32538345582499772, 67.03307707865299392, 5.290582662559629945 ) ) ;
#12722 = CARTESIAN_POINT ( 'NONE',  ( 77.26841646078648296, 67.71923746528655386, -25.22008900393981179 ) ) ;
#12723 = ORIENTED_EDGE ( 'NONE', *, *, #10534, .F. ) ;
#12724 = LINE ( 'NONE', #14014, #5301 ) ;
#12725 = DIRECTION ( 'NONE',  ( -0.5000000000000047740, 0.8660254037844358210, 0.000000000000000000 ) ) ;
#12726 = LINE ( 'NONE', #11028, #6825 ) ;
#12727 = VERTEX_POINT ( 'NONE', #12937 ) ;
#12728 = CARTESIAN_POINT ( 'NONE',  ( 81.11374900390920573, 66.94010251607396356, 0.6002589370414413983 ) ) ;
#12729 = ORIENTED_EDGE ( 'NONE', *, *, #14736, .T. ) ;
#12730 = AXIS2_PLACEMENT_3D ( 'NONE', #12080, #8576, #11872 ) ;
#12731 = ORIENTED_EDGE ( 'NONE', *, *, #20148, .F. ) ;
#12732 = CARTESIAN_POINT ( 'NONE',  ( -3.601598805479791388, 64.25000000000000000, 3.829763509598321125 ) ) ;
#12733 = CARTESIAN_POINT ( 'NONE',  ( 219.3085917042504036, 36.99313401332681650, -17.45257705044830487 ) ) ;
#12734 = EDGE_CURVE ( 'NONE', #245, #10584, #12341, .T. ) ;
#12735 = CARTESIAN_POINT ( 'NONE',  ( -17.86792573809073303, 79.99987962855902879, -12.43445577838060245 ) ) ;
#12736 = SHAPE_DEFINITION_REPRESENTATION ( #8899, #14136 ) ;
#12737 = CARTESIAN_POINT ( 'NONE',  ( 32.36389338619004263, 157.9004617752989930, -12.50000000000000000 ) ) ;
#12738 = ORIENTED_EDGE ( 'NONE', *, *, #19974, .F. ) ;
#12739 = CARTESIAN_POINT ( 'NONE',  ( 10.49211908931699178, -10.00000000000000000, 0.000000000000000000 ) ) ;
#12740 = VECTOR ( 'NONE', #18077, 999.9999999999998863 ) ;
#12741 = CARTESIAN_POINT ( 'NONE',  ( 203.6701878702990598, 1.459728612827534855, -3.762296834228767928 ) ) ;
#12742 = CARTESIAN_POINT ( 'NONE',  ( 216.7607129495440859, 9.790366881806683352, -5.993340328401894013 ) ) ;
#12743 = CARTESIAN_POINT ( 'NONE',  ( -0.08752631476754749174, 62.68128730906327917, 2.340095601044604567 ) ) ;
#12744 = EDGE_CURVE ( 'NONE', #791, #12727, #18014, .T. ) ;
#12745 = AXIS2_PLACEMENT_3D ( 'NONE', #9510, #16511, #11223 ) ;
#12746 = ORIENTED_EDGE ( 'NONE', *, *, #9256, .T. ) ;
#12747 = ADVANCED_FACE ( 'NONE', ( #19901 ), #9827, .T. ) ;
#12748 = DIRECTION ( 'NONE',  ( 0.5000000000000045519, -0.8660254037844361541, -0.000000000000000000 ) ) ;
#12749 = DIRECTION ( 'NONE',  ( 0.8660254037844372643, 0.5000000000000027756, -0.000000000000000000 ) ) ;
#12750 = CIRCLE ( 'NONE', #7312, 5.000000000000000000 ) ;
#12751 = DIRECTION ( 'NONE',  ( -0.2961981327260293506, -0.1710100716628398243, -0.9396926207859056523 ) ) ;
#12752 = DIRECTION ( 'NONE',  ( 0.8645602258681711616, 0.4991540791356389728, -0.05814482891047952767 ) ) ;
#12753 = CARTESIAN_POINT ( 'NONE',  ( -13.51899739228861463, 20.09941697557067641, 4.999999999999990230 ) ) ;
#12754 = ORIENTED_EDGE ( 'NONE', *, *, #13114, .F. ) ;
#12755 = PLANE ( 'NONE',  #9135 ) ;
#12756 = CARTESIAN_POINT ( 'NONE',  ( 76.75377061793378175, 71.15635013821236043, 0.07322384800663080118 ) ) ;
#12757 = EDGE_CURVE ( 'NONE', #17954, #1364, #20011, .T. ) ;
#12758 = DIRECTION ( 'NONE',  ( -0.8660254037844378194, -0.5000000000000013323, -0.000000000000000000 ) ) ;
#12759 = CARTESIAN_POINT ( 'NONE',  ( -20.89897948556633978, 16.09941697557071905, 0.9999999999999991118 ) ) ;
#12761 = ORIENTED_EDGE ( 'NONE', *, *, #7207, .T. ) ;
#12760 = ORIENTED_EDGE ( 'NONE', *, *, #10117, .T. ) ;
#12762 = VERTEX_POINT ( 'NONE', #5475 ) ;
#12763 = VECTOR ( 'NONE', #16083, 1000.000000000000227 ) ;
#12764 = DIRECTION ( 'NONE',  ( 1.000000000000000000, 0.000000000000000000, 0.000000000000000000 ) ) ;
#12765 = UNCERTAINTY_MEASURE_WITH_UNIT (LENGTH_MEASURE( 1.000000000000000082E-05 ), #19260, 'distance_accuracy_value', 'NONE');
#12766 = ORIENTED_EDGE ( 'NONE', *, *, #2704, .F. ) ;
#12767 = EDGE_CURVE ( 'NONE', #9819, #8753, #9929, .T. ) ;
#12768 = CARTESIAN_POINT ( 'NONE',  ( 202.9975627544909003, 8.494395787541842324, -26.16494226148076052 ) ) ;
#12769 = ORIENTED_EDGE ( 'NONE', *, *, #856, .F. ) ;
#12770 = DIRECTION ( 'NONE',  ( 0.000000000000000000, 0.000000000000000000, -1.000000000000000000 ) ) ;
#12771 = CARTESIAN_POINT ( 'NONE',  ( -26.96929348833892703, 80.00000000026912517, -6.044438231901797742 ) ) ;
#12772 = CARTESIAN_POINT ( 'NONE',  ( 221.7231637720595074, 32.81097251334476539, -16.48323849494068227 ) ) ;
#12773 = VERTEX_POINT ( 'NONE', #8450 ) ;
#12774 = VERTEX_POINT ( 'NONE', #1799 ) ;
#12775 = EDGE_CURVE ( 'NONE', #10411, #3183, #19796, .T. ) ;
#12776 = DIRECTION ( 'NONE',  ( -0.8660254037844354880, -0.5000000000000055511, 0.000000000000000000 ) ) ;
#12777 = ORIENTED_EDGE ( 'NONE', *, *, #6374, .T. ) ;
#12778 = CARTESIAN_POINT ( 'NONE',  ( 227.9553588074475670, 39.88513931160575510, -14.00000000000005507 ) ) ;
#12779 = VECTOR ( 'NONE', #1061, 1000.000000000000114 ) ;
#12780 = CARTESIAN_POINT ( 'NONE',  ( 220.9606893667113638, 33.51376855353427686, -16.94731950718130520 ) ) ;
#12781 = VECTOR ( 'NONE', #8136, 1000.000000000000227 ) ;
#12782 = CARTESIAN_POINT ( 'NONE',  ( 221.4896362261276863, 32.59760571852110189, -15.81459191843843648 ) ) ;
#12783 = EDGE_CURVE ( 'NONE', #14727, #2960, #11754, .T. ) ;
#12784 = CARTESIAN_POINT ( 'NONE',  ( 203.8052576239561802, 8.960718637850693113, -2.195132782454258358 ) ) ;
#12785 = EDGE_CURVE ( 'NONE', #13537, #12472, #11653, .T. ) ;
#12786 = ORIENTED_EDGE ( 'NONE', *, *, #12149, .T. ) ;
#12787 = DIRECTION ( 'NONE',  ( 0.5000000000000007772, -0.8660254037844381525, 0.000000000000000000 ) ) ;
#12788 = VERTEX_POINT ( 'NONE', #11539 ) ;
#12789 = CARTESIAN_POINT ( 'NONE',  ( 209.2925290576059467, 30.87145858698718826, -12.01256274262992463 ) ) ;
#12790 = CARTESIAN_POINT ( 'NONE',  ( -15.99999999999999289, 9.999999999999994671, 0.000000000000000000 ) ) ;
#12791 = DIRECTION ( 'NONE',  ( -0.5000000000000054401, 0.8660254037844354880, -0.000000000000000000 ) ) ;
#12792 = EDGE_CURVE ( 'NONE', #5372, #15392, #13088, .T. ) ;
#12793 = CARTESIAN_POINT ( 'NONE',  ( 5.000000000000000000, -2.342598717236899386, 4.057500000000001883 ) ) ;
#12794 = AXIS2_PLACEMENT_3D ( 'NONE', #5570, #12062, #18527 ) ;
#12795 = ORIENTED_EDGE ( 'NONE', *, *, #1968, .F. ) ;
#12796 = VECTOR ( 'NONE', #9974, 1000.000000000000227 ) ;
#12797 = PLANE ( 'NONE',  #5720 ) ;
#12798 = ADVANCED_FACE ( 'NONE', ( #17913 ), #9898, .T. ) ;
#12799 = VERTEX_POINT ( 'NONE', #14953 ) ;
#12800 = DIRECTION ( 'NONE',  ( 0.5000000000000026645, -0.8660254037844370423, 0.000000000000000000 ) ) ;
#12801 = CARTESIAN_POINT ( 'NONE',  ( -4.278641067966838740, 51.99310020370139540, -4.954688218471713590 ) ) ;
#12802 = DIRECTION ( 'NONE',  ( -0.5000000000000054401, 0.8660254037844354880, -0.000000000000000000 ) ) ;
#12803 = EDGE_CURVE ( 'NONE', #5249, #8280, #6864, .T. ) ;
#12804 = DIRECTION ( 'NONE',  ( 0.8645602258681718277, 0.4991540791356398055, 0.05814482891046528212 ) ) ;
#12805 = CARTESIAN_POINT ( 'NONE',  ( 96.88087538439037871, 198.6134603144003847, 11.16343975192298466 ) ) ;
#12806 = EDGE_CURVE ( 'NONE', #10112, #578, #1803, .T. ) ;
#12807 = AXIS2_PLACEMENT_3D ( 'NONE', #20368, #10937, #9224 ) ;
#12809 = EDGE_LOOP ( 'NONE', ( #12695, #9716, #321, #8834 ) ) ;
#12808 = ORIENTED_EDGE ( 'NONE', *, *, #9633, .F. ) ;
#12810 = ORIENTED_EDGE ( 'NONE', *, *, #5014, .F. ) ;
#12811 = CARTESIAN_POINT ( 'NONE',  ( 0.000000000000000000, 1.759474945355379960, -3.047500000000001652 ) ) ;
#12812 = DIRECTION ( 'NONE',  ( 0.000000000000000000, -1.000000000000000000, 0.000000000000000000 ) ) ;
#12813 = VECTOR ( 'NONE', #10910, 1000.000000000000000 ) ;
#12814 = CARTESIAN_POINT ( 'NONE',  ( -4.127064941938266784, 79.99999999978183496, -3.927153389735459132 ) ) ;
#12815 = EDGE_CURVE ( 'NONE', #13335, #2368, #19898, .T. ) ;
#12816 = ORIENTED_EDGE ( 'NONE', *, *, #17135, .F. ) ;
#12817 = ORIENTED_EDGE ( 'NONE', *, *, #8061, .F. ) ;
#12818 = ORIENTED_EDGE ( 'NONE', *, *, #18145, .F. ) ;
#12819 = CARTESIAN_POINT ( 'NONE',  ( -20.28206330180632833, 63.53129375914073762, -2.582219875156735345 ) ) ;
#12820 = CARTESIAN_POINT ( 'NONE',  ( 5.000000000000004441, 6.938893903907228378E-15, 4.057500000000028528 ) ) ;
#12821 = CARTESIAN_POINT ( 'NONE',  ( 215.9755601355957424, 15.98724606906508683, -13.98704593443257771 ) ) ;
#12822 = CARTESIAN_POINT ( 'NONE',  ( -28.39001627391951388, 8.716765542848399662, 1.688643308777810992 ) ) ;
#12823 = ORIENTED_EDGE ( 'NONE', *, *, #13668, .F. ) ;
#12824 = ORIENTED_EDGE ( 'NONE', *, *, #6035, .T. ) ;
#12825 = FACE_OUTER_BOUND ( 'NONE', #9295, .T. ) ;
#12826 = CIRCLE ( 'NONE', #3659, 11.94520687646042667 ) ;
#12827 = CARTESIAN_POINT ( 'NONE',  ( 200.1945581936670635, 6.876080349810432146, -24.60216584133502238 ) ) ;
#12828 = AXIS2_PLACEMENT_3D ( 'NONE', #2677, #7318, #15206 ) ;
#12829 = CARTESIAN_POINT ( 'NONE',  ( -29.99999999999999645, 5.000000000000000000, 15.00000000000000000 ) ) ;
#12830 = CARTESIAN_POINT ( 'NONE',  ( -27.38197634705172234, 68.30950415664236175, 5.167706431871533113 ) ) ;
#12831 = CARTESIAN_POINT ( 'NONE',  ( 209.7177441667290339, 12.37429433490069997, -24.99940654434242759 ) ) ;
#12832 = CARTESIAN_POINT ( 'NONE',  ( 217.5682316584538682, 37.87617127834120367, -14.91677899116112371 ) ) ;
#12833 = DIRECTION ( 'NONE',  ( -0.1005394128318207181, -0.05804645706261944010, -0.9932383577419421350 ) ) ;
#12834 = LINE ( 'NONE', #11243, #46 ) ;
#12835 = ORIENTED_EDGE ( 'NONE', *, *, #6255, .T. ) ;
#12836 = CARTESIAN_POINT ( 'NONE',  ( 66.21520157169484833, 72.86177730317662338, -2.126289421695329640 ) ) ;
#12837 = EDGE_LOOP ( 'NONE', ( #3218, #10648, #2043, #4326 ) ) ;
#12838 = VECTOR ( 'NONE', #20274, 1000.000000000000000 ) ;
#12839 = VERTEX_POINT ( 'NONE', #521 ) ;
#12840 = FACE_OUTER_BOUND ( 'NONE', #4547, .T. ) ;
#12841 = DIRECTION ( 'NONE',  ( -0.5000000000000051070, 0.8660254037844359321, -0.000000000000000000 ) ) ;
#12842 = ADVANCED_FACE ( 'NONE', ( #1899 ), #13658, .T. ) ;
#12843 = CARTESIAN_POINT ( 'NONE',  ( 205.5718816476997688, 14.10467741091863658, -2.341985411377013548 ) ) ;
#12844 = B_SPLINE_CURVE_WITH_KNOTS ( 'NONE', 3,
 ( #9112, #15614, #6998, #11136, #12732, #1494, #4360, #7941, #2778, #16032, #9219, #6344, #14443, #5932 ),
 .UNSPECIFIED., .F., .F.,
 ( 4, 2, 2, 2, 2, 2, 4 ),
 ( 0.000000000000000000, 0.001404861450950275039, 0.002107292176425411365, 0.002809722901900548343, 0.003512153627375684886, 0.004214584352850820996, 0.005619445803801094083 ),
 .UNSPECIFIED. ) ;
#12845 = SHAPE_DEFINITION_REPRESENTATION ( #10051, #10571 ) ;
#12846 = LINE ( 'NONE', #14664, #6539 ) ;
#12847 = ORIENTED_EDGE ( 'NONE', *, *, #5122, .T. ) ;
#12848 = FILL_AREA_STYLE ('',( #14451 ) ) ;
#12849 = APPLICATION_CONTEXT ( 'automotive_design' ) ;
#12850 = PLANE ( 'NONE',  #20265 ) ;
#12851 = CARTESIAN_POINT ( 'NONE',  ( 209.0112450435238145, 31.54208512462550118, -15.10854341765127806 ) ) ;
#12852 = DIRECTION ( 'NONE',  ( -0.8660254037844360431, -0.5000000000000045519, -0.000000000000000000 ) ) ;
#12853 = VECTOR ( 'NONE', #19813, 1000.000000000000000 ) ;
#12854 = CARTESIAN_POINT ( 'NONE',  ( 9.999999999999994671, 9.242062880866249359E-16, -8.000000000000000000 ) ) ;
#12855 = CARTESIAN_POINT ( 'NONE',  ( 1.500000000000001332, 0.000000000000000000, 0.000000000000000000 ) ) ;
#12856 = LINE ( 'NONE', #10640, #709 ) ;
#12857 = ADVANCED_FACE ( 'NONE', ( #3372 ), #17713, .T. ) ;
#12858 = DIRECTION ( 'NONE',  ( -0.8660254037844370423, -0.5000000000000026645, 0.000000000000000000 ) ) ;
#12859 = LINE ( 'NONE', #11361, #3091 ) ;
#12860 = ORIENTED_EDGE ( 'NONE', *, *, #1129, .F. ) ;
#12861 = FACE_BOUND ( 'NONE', #7361, .T. ) ;
#12862 = CARTESIAN_POINT ( 'NONE',  ( 81.23367086208386922, 54.81645704650414785, -2.629400372493356119 ) ) ;
#12863 = DIRECTION ( 'NONE',  ( 0.000000000000000000, 0.000000000000000000, -1.000000000000000000 ) ) ;
#12864 = CYLINDRICAL_SURFACE ( 'NONE', #5343, 11.99999999999999822 ) ;
#12865 = EDGE_CURVE ( 'NONE', #10626, #10118, #20403, .T. ) ;
#12867 = ORIENTED_EDGE ( 'NONE', *, *, #9003, .T. ) ;
#12866 = ORIENTED_EDGE ( 'NONE', *, *, #2110, .T. ) ;
#12868 = EDGE_CURVE ( 'NONE', #3652, #16112, #9267, .T. ) ;
#12869 = DIRECTION ( 'NONE',  ( 0.000000000000000000, 0.000000000000000000, 1.000000000000000000 ) ) ;
#12870 = ORIENTED_EDGE ( 'NONE', *, *, #10445, .T. ) ;
#12871 = AXIS2_PLACEMENT_3D ( 'NONE', #14619, #16295, #1561 ) ;
#12872 = DIRECTION ( 'NONE',  ( -0.8660254037844360431, -0.5000000000000044409, -4.336808689942049290E-16 ) ) ;
#12873 = ORIENTED_EDGE ( 'NONE', *, *, #8233, .T. ) ;
#12874 = CARTESIAN_POINT ( 'NONE',  ( 196.8389703229736938, 4.584704208019711125, -20.76014333877581564 ) ) ;
#12875 = CARTESIAN_POINT ( 'NONE',  ( -28.46762626707359445, 79.99999999989459809, -0.9530258780664238039 ) ) ;
#12876 = CARTESIAN_POINT ( 'NONE',  ( 198.4557123656591386, 5.695147338747302612, -22.83852658738919317 ) ) ;
#12877 = VERTEX_POINT ( 'NONE', #13985 ) ;
#12878 = FACE_OUTER_BOUND ( 'NONE', #18852, .T. ) ;
#12879 = CARTESIAN_POINT ( 'NONE',  ( 193.0882619218634488, 6.897256201746025717, -18.44761907388178557 ) ) ;
#12880 = PRODUCT_DEFINITION ( 'UNKNOWN', '', #986, #20391 ) ;
#12881 = DIRECTION ( 'NONE',  ( -0.000000000000000000, -1.000000000000000000, -0.000000000000000000 ) ) ;
#12882 = ORIENTED_EDGE ( 'NONE', *, *, #19159, .T. ) ;
#12883 = AXIS2_PLACEMENT_3D ( 'NONE', #6365, #1202, #7654 ) ;
#12884 = CARTESIAN_POINT ( 'NONE',  ( 203.8353993890810898, 8.978120994059423765, -2.341985411376945159 ) ) ;
#12885 = DIRECTION ( 'NONE',  ( 0.000000000000000000, 0.9841898184435641239, 0.1771169141330785901 ) ) ;
#12886 = AXIS2_PLACEMENT_3D ( 'NONE', #13719, #786, #10406 ) ;
#12887 = ORIENTED_EDGE ( 'NONE', *, *, #15373, .F. ) ;
#12888 = DIRECTION ( 'NONE',  ( 0.000000000000000000, 0.000000000000000000, -1.000000000000000000 ) ) ;
#12889 = VECTOR ( 'NONE', #15179, 1000.000000000000114 ) ;
#12890 = EDGE_CURVE ( 'NONE', #425, #9243, #3714, .T. ) ;
#12891 = ORIENTED_EDGE ( 'NONE', *, *, #18809, .T. ) ;
#12892 = CARTESIAN_POINT ( 'NONE',  ( 208.9194833127196489, 31.78152281641241572, -13.67345714572792659 ) ) ;
#12893 = CARTESIAN_POINT ( 'NONE',  ( 216.6298941398503359, 15.83397672076898566, -14.01558723443205068 ) ) ;
#12894 = DIRECTION ( 'NONE',  ( -0.8660254037844362651, -0.5000000000000043299, 0.000000000000000000 ) ) ;
#12895 = VECTOR ( 'NONE', #5188, 1000.000000000000227 ) ;
#12896 = VECTOR ( 'NONE', #10721, 1000.000000000000227 ) ;
#12897 = CARTESIAN_POINT ( 'NONE',  ( 209.0908153953612612, 5.362149464242316199, -1.545471579934816875 ) ) ;
#12898 = CARTESIAN_POINT ( 'NONE',  ( -29.99999999999963052, 5.000000000000220268, -4.654981692112267311 ) ) ;
#12899 = VECTOR ( 'NONE', #4539, 1000.000000000000227 ) ;
#12900 = EDGE_LOOP ( 'NONE', ( #8357, #16863, #19396, #20584, #10784, #10675, #4007, #16738, #3052, #7348, #8177, #14608 ) ) ;
#12901 = VECTOR ( 'NONE', #5735, 1000.000000000000227 ) ;
#12902 = EDGE_CURVE ( 'NONE', #18515, #7908, #1127, .T. ) ;
#12903 = DIRECTION ( 'NONE',  ( -0.8660254037844378194, -0.5000000000000013323, -0.000000000000000000 ) ) ;
#12904 = CIRCLE ( 'NONE', #4443, 5.400000000000040323 ) ;
#12905 = DIRECTION ( 'NONE',  ( -0.8660254037844362651, -0.5000000000000042188, 0.000000000000000000 ) ) ;
#12906 = CARTESIAN_POINT ( 'NONE',  ( -0.8702360668455834114, 50.25436005864763445, -9.730529323853312818 ) ) ;
#12907 = DIRECTION ( 'NONE',  ( 0.000000000000000000, 0.000000000000000000, -1.000000000000000000 ) ) ;
#12908 = ADVANCED_FACE ( 'NONE', ( #1039 ), #8775, .T. ) ;
#12909 = AXIS2_PLACEMENT_3D ( 'NONE', #19983, #1975, #11832 ) ;
#12910 = DIRECTION ( 'NONE',  ( -0.5000000000000049960, 0.8660254037844357100, 0.000000000000000000 ) ) ;
#12911 = DIRECTION ( 'NONE',  ( -0.5000000000000051070, 0.8660254037844359321, -0.000000000000000000 ) ) ;
#12913 = EDGE_LOOP ( 'NONE', ( #6495, #17071, #19830, #746 ) ) ;
#12912 = VERTEX_POINT ( 'NONE', #13664 ) ;
#12914 = VECTOR ( 'NONE', #4684, 1000.000000000000000 ) ;
#12915 = LINE ( 'NONE', #13224, #16616 ) ;
#12916 = CARTESIAN_POINT ( 'NONE',  ( 198.0085843809688413, -1.293793446905138422, -15.42246552719588948 ) ) ;
#12917 = EDGE_CURVE ( 'NONE', #10655, #7353, #9179, .T. ) ;
#12918 = CARTESIAN_POINT ( 'NONE',  ( -2.526178703648428669, 77.46132694877630342, -4.041171758127903857 ) ) ;
#12919 = VECTOR ( 'NONE', #5217, 1000.000000000000000 ) ;
#12920 = VERTEX_POINT ( 'NONE', #4321 ) ;
#12921 = ORIENTED_EDGE ( 'NONE', *, *, #17958, .T. ) ;
#12922 = CARTESIAN_POINT ( 'NONE',  ( -19.54621117075676651, 60.56420712653811478, -3.531915534904321419 ) ) ;
#12923 = DIRECTION ( 'NONE',  ( 1.060575238724903710E-16, 6.123233995736822735E-17, 1.000000000000000000 ) ) ;
#12924 = SPHERICAL_SURFACE ( 'NONE', #2072, 12.00000000000002665 ) ;
#12925 = PLANE ( 'NONE',  #6636 ) ;
#12926 = ORIENTED_EDGE ( 'NONE', *, *, #17508, .T. ) ;
#12927 = ORIENTED_EDGE ( 'NONE', *, *, #1889, .T. ) ;
#12928 = CARTESIAN_POINT ( 'NONE',  ( 195.1138010445122575, 8.066701759461459176, -22.49869731917958049 ) ) ;
#12929 = ADVANCED_FACE ( 'NONE', ( #16836 ), #5682, .F. ) ;
#12930 = CIRCLE ( 'NONE', #59, 12.99999999999999822 ) ;
#12931 = ADVANCED_FACE ( 'NONE', ( #15376 ), #5892, .T. ) ;
#12932 = DIRECTION ( 'NONE',  ( -0.8601696498176548689, -0.4966191788709768407, 0.1160929141252376451 ) ) ;
#12933 = AXIS2_PLACEMENT_3D ( 'NONE', #14049, #12352, #15436 ) ;
#12934 = CIRCLE ( 'NONE', #19351, 11.00000000000001066 ) ;
#12935 = CARTESIAN_POINT ( 'NONE',  ( 221.1038914607097183, 33.88358362032316506, -10.52303454827242213 ) ) ;
#12936 = FACE_OUTER_BOUND ( 'NONE', #19926, .T. ) ;
#12937 = CARTESIAN_POINT ( 'NONE',  ( 213.9513496856694132, 7.395560154513789897, -3.762296834228892717 ) ) ;
#12938 = AXIS2_PLACEMENT_3D ( 'NONE', #12778, #4812, #17227 ) ;
#12939 = ADVANCED_FACE ( 'NONE', ( #10568 ), #12172, .F. ) ;
#12940 = CARTESIAN_POINT ( 'NONE',  ( 229.0531201841587574, 37.00429494149224752, -11.55788255683065735 ) ) ;
#12941 = CARTESIAN_POINT ( 'NONE',  ( 218.1288387380593576, 38.20904687787225384, -14.00000000000005507 ) ) ;
#12942 = ORIENTED_EDGE ( 'NONE', *, *, #9378, .F. ) ;
#12943 = CARTESIAN_POINT ( 'NONE',  ( 65.99961509271065552, 79.76980348214863170, -3.334180729184369696 ) ) ;
#12944 = ORIENTED_EDGE ( 'NONE', *, *, #13888, .F. ) ;
#12945 = ORIENTED_EDGE ( 'NONE', *, *, #10824, .F. ) ;
#12946 = CARTESIAN_POINT ( 'NONE',  ( 31.00000000000000711, 65.00000000000000000, -22.49999999999999645 ) ) ;
#12947 = CARTESIAN_POINT ( 'NONE',  ( 225.7363529196993568, 42.74910436041706419, -12.46964089162983313 ) ) ;
#12948 = EDGE_CURVE ( 'NONE', #12454, #15941, #1151, .T. ) ;
#12949 = VECTOR ( 'NONE', #9874, 1000.000000000000227 ) ;
#12950 = VECTOR ( 'NONE', #19690, 1000.000000000000114 ) ;
#12951 = FACE_OUTER_BOUND ( 'NONE', #6657, .T. ) ;
#12952 = ORIENTED_EDGE ( 'NONE', *, *, #629, .F. ) ;
#12953 = DIRECTION ( 'NONE',  ( 0.5000000000000007772, -0.8660254037844381525, 0.000000000000000000 ) ) ;
#12954 = ITEM_DEFINED_TRANSFORMATION ( 'NONE', 'NONE', #9412,  #18233 ) ;
#12955 = B_SPLINE_CURVE_WITH_KNOTS ( 'NONE', 3,
 ( #17456, #14299, #9376, #19052 ),
 .UNSPECIFIED., .F., .F.,
 ( 4, 4 ),
 ( 0.0001275232718639688831, 0.0008001740639077388690 ),
 .UNSPECIFIED. ) ;
#12956 = CARTESIAN_POINT ( 'NONE',  ( 80.00000000000000000, 0.000000000000000000, 0.000000000000000000 ) ) ;
#12957 = ORIENTED_EDGE ( 'NONE', *, *, #1196, .T. ) ;
#12958 = CARTESIAN_POINT ( 'NONE',  ( 215.7669897261582435, 15.51280130567490367, -9.783550055872625606 ) ) ;
#12959 = CARTESIAN_POINT ( 'NONE',  ( 211.3372400686716617, 27.55192669161114694, -14.80705122880212166 ) ) ;
#12960 = PLANE ( 'NONE',  #13578 ) ;
#12961 = CARTESIAN_POINT ( 'NONE',  ( 215.5386005439712562, 15.73496733121568170, -17.74130751083515634 ) ) ;
#12962 = DIRECTION ( 'NONE',  ( 0.5000000000000052180, -0.8660254037844355990, -5.551115123125782086E-17 ) ) ;
#12963 = CIRCLE ( 'NONE', #11590, 5.999999999999998224 ) ;
#12964 = CARTESIAN_POINT ( 'NONE',  ( 209.4137679361615767, 3.391338277461352302, -14.00000000000005507 ) ) ;
#12965 = VECTOR ( 'NONE', #9902, 1000.000000000000227 ) ;
#12966 = CARTESIAN_POINT ( 'NONE',  ( 205.5254235590770406, 9.953856903543574219, -12.15027190984248229 ) ) ;
#12967 = DIRECTION ( 'NONE',  ( 0.5000000000000049960, -0.8660254037844358210, 0.000000000000000000 ) ) ;
#12968 = ORIENTED_EDGE ( 'NONE', *, *, #17337, .F. ) ;
#12969 = ORIENTED_EDGE ( 'NONE', *, *, #6831, .F. ) ;
#12970 = DIRECTION ( 'NONE',  ( 0.000000000000000000, 1.000000000000000000, -1.302777330458572662E-15 ) ) ;
#12971 = CARTESIAN_POINT ( 'NONE',  ( 82.41701720340896031, 64.90144913130031057, 0.6268774674042598694 ) ) ;
#12972 = CARTESIAN_POINT ( 'NONE',  ( 54.65554463217808490, 249.2901892326410689, -13.99999999999998046 ) ) ;
#12973 = CARTESIAN_POINT ( 'NONE',  ( 75.04800910938280367, 52.02334688640443972, -11.56191590910611389 ) ) ;
#12975 = ORIENTED_EDGE ( 'NONE', *, *, #20804, .T. ) ;
#12974 = ORIENTED_EDGE ( 'NONE', *, *, #3950, .T. ) ;
#12976 = PRESENTATION_STYLE_ASSIGNMENT (( #9453 ) ) ;
#12977 = UNCERTAINTY_MEASURE_WITH_UNIT (LENGTH_MEASURE( 1.000000000000000082E-05 ), #9407, 'distance_accuracy_value', 'NONE');
#12978 = ORIENTED_EDGE ( 'NONE', *, *, #20424, .F. ) ;
#12979 = CIRCLE ( 'NONE', #3818, 9.999999999999998224 ) ;
#12980 = CARTESIAN_POINT ( 'NONE',  ( 221.8610514736063806, 32.16021383998725014, -14.54260449067782623 ) ) ;
#12981 = ORIENTED_EDGE ( 'NONE', *, *, #18965, .F. ) ;
#12982 = DIRECTION ( 'NONE',  ( -0.8660254037844361541, -0.5000000000000045519, 5.976026924694053325E-17 ) ) ;
#12983 = CARTESIAN_POINT ( 'NONE',  ( -28.78765050820362603, 78.65050410969298866, -6.103909342518194059 ) ) ;
#12984 = CARTESIAN_POINT ( 'NONE',  ( 195.4998201364199417, 4.165572068683992768, -11.22353489230383339 ) ) ;
#12985 = CARTESIAN_POINT ( 'NONE',  ( -15.99999999999999289, 64.25000000000000000, 0.000000000000000000 ) ) ;
#12986 = CARTESIAN_POINT ( 'NONE',  ( 56.32485119810130669, 77.11604862365510371, -17.22740159993880482 ) ) ;
#12987 = EDGE_CURVE ( 'NONE', #8117, #10684, #4004, .T. ) ;
#12988 = CARTESIAN_POINT ( 'NONE',  ( -29.98143750865132162, 64.25000000000000000, 2.826871295670245310 ) ) ;
#12989 = ORIENTED_EDGE ( 'NONE', *, *, #15267, .T. ) ;
#12990 = CIRCLE ( 'NONE', #13671, 11.98469917212512215 ) ;
#12991 = DIRECTION ( 'NONE',  ( -0.5000000000000057732, 0.8660254037844352659, 0.000000000000000000 ) ) ;
#12992 = DIRECTION ( 'NONE',  ( -0.1674398060854888903, 0.2900142513495467256, -0.9422609221188237294 ) ) ;
#12993 = VERTEX_POINT ( 'NONE', #18638 ) ;
#12994 = CARTESIAN_POINT ( 'NONE',  ( 226.1688508298258853, 42.97946189697395170, -13.95097276009431297 ) ) ;
#12995 = VERTEX_POINT ( 'NONE', #15271 ) ;
#12996 = DIRECTION ( 'NONE',  ( -0.5000000000000051070, 0.8660254037844359321, -0.000000000000000000 ) ) ;
#12997 = DIRECTION ( 'NONE',  ( 0.000000000000000000, 0.000000000000000000, -1.000000000000000000 ) ) ;
#12998 = CARTESIAN_POINT ( 'NONE',  ( 205.8264633344831225, 9.596613037118636669, -14.00000000000005507 ) ) ;
#12999 = EDGE_CURVE ( 'NONE', #918, #13886, #13999, .T. ) ;
#13000 = FACE_OUTER_BOUND ( 'NONE', #6376, .T. ) ;
#13001 = CARTESIAN_POINT ( 'NONE',  ( 159.9952905943347901, 46.83639716978954226, -6.000000000000052403 ) ) ;
#13002 = CIRCLE ( 'NONE', #20432, 11.94520687646042667 ) ;
#13003 = AXIS2_PLACEMENT_3D ( 'NONE', #11890, #12095, #14015 ) ;
#13004 = DIRECTION ( 'NONE',  ( 0.000000000000000000, -0.9557539690135837818, -0.2941672155675774669 ) ) ;
#13005 = EDGE_LOOP ( 'NONE', ( #2703, #10457, #17, #19373, #19266, #13484 ) ) ;
#13006 = CARTESIAN_POINT ( 'NONE',  ( 69.47824080215001175, 71.42279538029322339, -23.81892892278162677 ) ) ;
#13007 = LINE ( 'NONE', #11405, #17604 ) ;
#13008 = ADVANCED_FACE ( 'NONE', ( #16938 ), #4113, .T. ) ;
#13009 = ORIENTED_EDGE ( 'NONE', *, *, #15881, .F. ) ;
#13010 = EDGE_CURVE ( 'NONE', #4238, #16527, #12979, .T. ) ;
#13011 = LINE ( 'NONE', #9696, #12965 ) ;
#13012 = CARTESIAN_POINT ( 'NONE',  ( -11.30699436262336022, 45.34934999665991029, -11.59074373136150271 ) ) ;
#13013 = DIRECTION ( 'NONE',  ( 0.000000000000000000, 0.000000000000000000, 1.000000000000000000 ) ) ;
#13014 = DIRECTION ( 'NONE',  ( 1.000000000000000000, 0.000000000000000000, 0.000000000000000000 ) ) ;
#13015 = CARTESIAN_POINT ( 'NONE',  ( -19.79889058375756861, 45.44132677019771904, -11.91506545529773753 ) ) ;
#13017 = ORIENTED_EDGE ( 'NONE', *, *, #6238, .T. ) ;
#13016 = ORIENTED_EDGE ( 'NONE', *, *, #2178, .F. ) ;
#13018 = ORIENTED_EDGE ( 'NONE', *, *, #9143, .F. ) ;
#13019 = VECTOR ( 'NONE', #19444, 1000.000000000000114 ) ;
#13020 = CARTESIAN_POINT ( 'NONE',  ( -20.40277896402405133, 11.66854079980773307, 3.430876175762952673 ) ) ;
#13021 = CARTESIAN_POINT ( 'NONE',  ( 198.5374064076044078, -1.503684146350823703, -15.40190399002796440 ) ) ;
#13022 = ORIENTED_EDGE ( 'NONE', *, *, #8091, .F. ) ;
#13023 = VERTEX_POINT ( 'NONE', #2635 ) ;
#13024 = EDGE_CURVE ( 'NONE', #9110, #8857, #9076, .T. ) ;
#13025 = CARTESIAN_POINT ( 'NONE',  ( 0.000000000000000000, -4.685197434473809430, 6.071532165918824830E-15 ) ) ;
#13026 = CARTESIAN_POINT ( 'NONE',  ( 10.00000000000000178, 0.000000000000000000, 0.000000000000000000 ) ) ;
#13027 = DIRECTION ( 'NONE',  ( 0.5000000000000039968, -0.8660254037844362651, 0.000000000000000000 ) ) ;
#13028 = CARTESIAN_POINT ( 'NONE',  ( 208.4761278624580711, 5.007259451653140125, -14.00000000000005507 ) ) ;
#13029 = EDGE_LOOP ( 'NONE', ( #6614, #11083, #17217, #15197 ) ) ;
#13030 = ORIENTED_EDGE ( 'NONE', *, *, #13963, .F. ) ;
#13031 = DIRECTION ( 'NONE',  ( 0.5000000000000034417, -0.8660254037844364872, 0.000000000000000000 ) ) ;
#13032 = B_SPLINE_CURVE_WITH_KNOTS ( 'NONE', 3,
 ( #15005, #2257, #6906, #5306 ),
 .UNSPECIFIED., .F., .F.,
 ( 4, 4 ),
 ( 3.577803810849139650E-07, 0.0006730085724363164519 ),
 .UNSPECIFIED. ) ;
#13033 = EDGE_CURVE ( 'NONE', #6749, #13669, #6509, .T. ) ;
#13034 = AXIS2_PLACEMENT_3D ( 'NONE', #4602, #4506, #1010 ) ;
#13035 = CARTESIAN_POINT ( 'NONE',  ( 207.4098631234038521, 11.04183859327925354, -25.80036831778744144 ) ) ;
#13036 = EDGE_CURVE ( 'NONE', #10069, #17136, #11963, .T. ) ;
#13037 = CARTESIAN_POINT ( 'NONE',  ( 97.00490953756779788, 125.9389375482329569, 55.99999999999997868 ) ) ;
#13038 = CARTESIAN_POINT ( 'NONE',  ( -28.04417108971878037, 54.76469415528241313, 3.349407265930378408 ) ) ;
#13039 = CARTESIAN_POINT ( 'NONE',  ( -20.93440336536924562, 15.92340406867066882, 11.48489954023713899 ) ) ;
#13040 = ORIENTED_EDGE ( 'NONE', *, *, #8412, .T. ) ;
#13041 = ADVANCED_FACE ( 'NONE', ( #16093 ), #3163, .T. ) ;
#13042 = DIRECTION ( 'NONE',  ( -0.5000000000000051070, 0.8660254037844359321, -0.000000000000000000 ) ) ;
#13043 = CARTESIAN_POINT ( 'NONE',  ( 205.0193973458067092, 9.661702533094931766, -25.81526893633797570 ) ) ;
#13044 = EDGE_LOOP ( 'NONE', ( #10040, #6039, #8674, #8292 ) ) ;
#13045 = ORIENTED_EDGE ( 'NONE', *, *, #20153, .F. ) ;
#13046 = CARTESIAN_POINT ( 'NONE',  ( 64.14641058282846586, 81.20660516694680098, -4.421514697542901828 ) ) ;
#13047 = ADVANCED_FACE ( 'NONE', ( #12489 ), #18945, .F. ) ;
#13048 = EDGE_LOOP ( 'NONE', ( #7934, #8327, #14099, #16372 ) ) ;
#13049 = EDGE_CURVE ( 'NONE', #16451, #184, #5519, .T. ) ;
#13050 = DIRECTION ( 'NONE',  ( 0.000000000000000000, -0.5000000000000018874, -0.8660254037844374864 ) ) ;
#13051 = VECTOR ( 'NONE', #13742, 1000.000000000000114 ) ;
#13052 = VERTEX_POINT ( 'NONE', #20936 ) ;
#13053 = DIRECTION ( 'NONE',  ( -0.8660254037844370423, -0.5000000000000026645, 0.000000000000000000 ) ) ;
#13054 = ADVANCED_FACE ( 'NONE', ( #19058 ), #11204, .F. ) ;
#13055 = DIRECTION ( 'NONE',  ( 1.000000000000000000, -0.000000000000000000, -0.000000000000000000 ) ) ;
#13056 = ORIENTED_EDGE ( 'NONE', *, *, #3301, .T. ) ;
#13057 = DIRECTION ( 'NONE',  ( 0.8660254037844360431, 0.5000000000000044409, -5.976026924694052093E-17 ) ) ;
#13058 = CARTESIAN_POINT ( 'NONE',  ( 211.4194833127197342, 27.45139579749024605, -14.16549164512199965 ) ) ;
#13059 = FACE_OUTER_BOUND ( 'NONE', #15393, .T. ) ;
#13060 = DIRECTION ( 'NONE',  ( -0.5000000000000049960, 0.8660254037844357100, -0.000000000000000000 ) ) ;
#13061 = EDGE_CURVE ( 'NONE', #14523, #20133, #17466, .T. ) ;
#13062 = DIRECTION ( 'NONE',  ( -0.8660254037844380415, -0.5000000000000014433, -0.000000000000000000 ) ) ;
#13063 = DIRECTION ( 'NONE',  ( -0.5000000000000049960, 0.8660254037844357100, -0.000000000000000000 ) ) ;
#13064 = CARTESIAN_POINT ( 'NONE',  ( 220.0968443491207722, 35.00999201386641602, -10.43865930680574827 ) ) ;
#13065 = CIRCLE ( 'NONE', #10662, 7.155882939242646401 ) ;
#13066 = ORIENTED_EDGE ( 'NONE', *, *, #10815, .F. ) ;
#13067 = AXIS2_PLACEMENT_3D ( 'NONE', #10266, #3703, #327 ) ;
#13068 = ORIENTED_EDGE ( 'NONE', *, *, #1389, .T. ) ;
#13069 = CARTESIAN_POINT ( 'NONE',  ( 200.3972727712213668, 6.993117665730062882, -3.627429155984474907 ) ) ;
#13070 = ADVANCED_FACE ( 'NONE', ( #15993, #1251 ), #1458, .T. ) ;
#13071 = CARTESIAN_POINT ( 'NONE',  ( 58.87500628332524855, 85.27019789096429747, -10.51825745130593859 ) ) ;
#13072 = ORIENTED_EDGE ( 'NONE', *, *, #7047, .T. ) ;
#13073 = CARTESIAN_POINT ( 'NONE',  ( -15.11015962792897227, 71.52657754998247697, -4.923257761629217910 ) ) ;
#13074 = CARTESIAN_POINT ( 'NONE',  ( 79.63536887191790470, 50.25278888007263589, -8.464988250521633617 ) ) ;
#13076 = ORIENTED_EDGE ( 'NONE', *, *, #3785, .F. ) ;
#13075 = ORIENTED_EDGE ( 'NONE', *, *, #9615, .F. ) ;
#13077 = VERTEX_POINT ( 'NONE', #7904 ) ;
#13078 = EDGE_LOOP ( 'NONE', ( #11004, #16390, #11842, #16805 ) ) ;
#13079 = CONICAL_SURFACE ( 'NONE', #9667, 10.85470691220533190, 0.8171114040043576665 ) ;
#13080 = CARTESIAN_POINT ( 'NONE',  ( 222.1491677973493495, 32.07311189731386492, -14.55761806292095706 ) ) ;
#13081 = ORIENTED_EDGE ( 'NONE', *, *, #9977, .T. ) ;
#13082 = CIRCLE ( 'NONE', #12063, 11.50000000000002665 ) ;
#13083 = SURFACE_STYLE_FILL_AREA ( #14790 ) ;
#13084 = VECTOR ( 'NONE', #14621, 999.9999999999998863 ) ;
#13085 = CARTESIAN_POINT ( 'NONE',  ( -28.23783794168646466, 80.00000000009136158, -2.568690455535888262 ) ) ;
#13086 = DIRECTION ( 'NONE',  ( 0.5000000000000054401, -0.8660254037844354880, 0.000000000000000000 ) ) ;
#13087 = B_SPLINE_CURVE_WITH_KNOTS ( 'NONE', 3,
 ( #3367, #9822, #1794, #8235 ),
 .UNSPECIFIED., .F., .F.,
 ( 4, 4 ),
 ( 5.020066588672724092E-07, 0.0005859903623984725508 ),
 .UNSPECIFIED. ) ;
#13088 = B_SPLINE_CURVE_WITH_KNOTS ( 'NONE', 3,
 ( #3484, #16733, #8238, #622 ),
 .UNSPECIFIED., .F., .F.,
 ( 4, 4 ),
 ( 8.130009260133085402E-07, 0.0008547987389031481238 ),
 .UNSPECIFIED. ) ;
#13089 = DIRECTION ( 'NONE',  ( 0.000000000000000000, 1.000000000000000000, -1.232415585510385534E-15 ) ) ;
#13090 = CARTESIAN_POINT ( 'NONE',  ( 54.44419410798747094, 77.91572085402148673, -11.00332497362847661 ) ) ;
#13091 = CARTESIAN_POINT ( 'NONE',  ( 75.60317707801357301, 163.0078255381764905, 41.00000000000001421 ) ) ;
#13092 = ORIENTED_EDGE ( 'NONE', *, *, #9205, .F. ) ;
#13093 = CIRCLE ( 'NONE', #7319, 11.98469917212512215 ) ;
#13094 = FILL_AREA_STYLE_COLOUR ( '', #11526 ) ;
#13095 = DIRECTION ( 'NONE',  ( 0.000000000000000000, 0.9557539690135837818, 0.2941672155675774669 ) ) ;
#13096 = CIRCLE ( 'NONE', #10358, 12.47473710546057823 ) ;
#13097 = EDGE_LOOP ( 'NONE', ( #6341, #4378, #14209, #11874, #4693, #16408, #8499, #1792 ) ) ;
#13098 = DIRECTION ( 'NONE',  ( 0.000000000000000000, -1.000000000000000000, 0.000000000000000000 ) ) ;
#13099 = VERTEX_POINT ( 'NONE', #10998 ) ;
#13100 = CARTESIAN_POINT ( 'NONE',  ( 205.0662616026534693, 10.91332106064940888, -14.00000000000005507 ) ) ;
#13101 = CYLINDRICAL_SURFACE ( 'NONE', #7139, 12.50000000000000000 ) ;
#13102 = FACE_OUTER_BOUND ( 'NONE', #10865, .T. ) ;
#13103 = PLANE ( 'NONE',  #20172 ) ;
#13104 = EDGE_CURVE ( 'NONE', #12601, #5435, #17365, .T. ) ;
#13105 = DIRECTION ( 'NONE',  ( -0.4953429730181667656, 0.8579591964396799941, -0.1361666490962538667 ) ) ;
#13106 = FACE_OUTER_BOUND ( 'NONE', #1938, .T. ) ;
#13107 = ORIENTED_EDGE ( 'NONE', *, *, #6581, .F. ) ;
#13108 = AXIS2_PLACEMENT_3D ( 'NONE', #7931, #5923, #9523 ) ;
#13109 = CARTESIAN_POINT ( 'NONE',  ( -15.22417136430887119, 45.62850095463065259, -12.48193588431748324 ) ) ;
#13110 = DIRECTION ( 'NONE',  ( 0.000000000000000000, 0.4999999999999985012, -0.8660254037844394848 ) ) ;
#13111 = CARTESIAN_POINT ( 'NONE',  ( -0.01127596767515291407, 61.98808745880752724, 2.211961002137901922 ) ) ;
#13112 = DIRECTION ( 'NONE',  ( -0.000000000000000000, -1.000000000000000000, -0.000000000000000000 ) ) ;
#13113 = CARTESIAN_POINT ( 'NONE',  ( 9.999999999999998224, 8.000000000000000000, 0.000000000000000000 ) ) ;
#13114 = EDGE_CURVE ( 'NONE', #13972, #527, #14066, .T. ) ;
#13115 = CARTESIAN_POINT ( 'NONE',  ( 208.9187556984696812, 16.03699604507445287, -24.25943249057096907 ) ) ;
#13116 = VERTEX_POINT ( 'NONE', #15783 ) ;
#13117 = ORIENTED_EDGE ( 'NONE', *, *, #3087, .T. ) ;
#13118 = CARTESIAN_POINT ( 'NONE',  ( 221.5793113145849134, 32.44228390914006610, -15.46846178913030201 ) ) ;
#13119 = CARTESIAN_POINT ( 'NONE',  ( 0.000000000000000000, -2.342598717236899830, 4.057500000000059615 ) ) ;
#13120 = ORIENTED_EDGE ( 'NONE', *, *, #17701, .T. ) ;
#13121 = ORIENTED_EDGE ( 'NONE', *, *, #13190, .T. ) ;
#13122 = AXIS2_PLACEMENT_3D ( 'NONE', #5158, #15370, #821 ) ;
#13123 = CARTESIAN_POINT ( 'NONE',  ( -17.39810202520303406, 58.61478893848392602, -4.803508630518933842 ) ) ;
#13124 = CARTESIAN_POINT ( 'NONE',  ( 9.999999999999994671, 0.000000000000000000, 0.000000000000000000 ) ) ;
#13125 = CARTESIAN_POINT ( 'NONE',  ( 86.00000000000000000, 65.00000000000000000, -25.50000000000000000 ) ) ;
#13126 = CARTESIAN_POINT ( 'NONE',  ( 195.2863413965735333, 4.042320060767385037, -12.62152863576138806 ) ) ;
#13127 = ORIENTED_EDGE ( 'NONE', *, *, #941, .F. ) ;
#13128 = EDGE_CURVE ( 'NONE', #7006, #6033, #19406, .T. ) ;
#13129 = AXIS2_PLACEMENT_3D ( 'NONE', #18924, #6286, #17441 ) ;
#13130 = VERTEX_POINT ( 'NONE', #17774 ) ;
#13131 = ADVANCED_FACE ( 'NONE', ( #7802 ), #14403, .T. ) ;
#13132 = CARTESIAN_POINT ( 'NONE',  ( 215.4868200432858600, 15.17402258341379451, -8.415281845792092597 ) ) ;
#13133 = B_SPLINE_CURVE_WITH_KNOTS ( 'NONE', 3,
 ( #15808, #6127, #17594, #20759 ),
 .UNSPECIFIED., .F., .F.,
 ( 4, 4 ),
 ( 3.531115201800005611E-07, 0.0004524063533000636616 ),
 .UNSPECIFIED. ) ;
#13134 = LINE ( 'NONE', #18110, #13199 ) ;
#13135 = VECTOR ( 'NONE', #1451, 1000.000000000000227 ) ;
#13136 = CARTESIAN_POINT ( 'NONE',  ( 197.7335577521869823, 5.455221082446096936, -21.59012016402710188 ) ) ;
#13137 = CARTESIAN_POINT ( 'NONE',  ( -28.81347165278748790, 54.47717305474855465, -1.798637628744577555 ) ) ;
#13138 = CARTESIAN_POINT ( 'NONE',  ( -17.30956942029561674, 19.93606970371389764, 12.43541898840899940 ) ) ;
#13139 = VECTOR ( 'NONE', #10796, 1000.000000000000227 ) ;
#13140 = CARTESIAN_POINT ( 'NONE',  ( 57.15554463217811332, 244.9600622137188850, -13.99999999999998046 ) ) ;
#13141 = CARTESIAN_POINT ( 'NONE',  ( -15.99999999999999289, 0.000000000000000000, 5.999999999999989342 ) ) ;
#13142 = PRODUCT_DEFINITION ( 'UNKNOWN', '', #19263, #15547 ) ;
#13143 = VERTEX_POINT ( 'NONE', #3243 ) ;
#13144 = ORIENTED_EDGE ( 'NONE', *, *, #12238, .F. ) ;
#13146 = EDGE_CURVE ( 'NONE', #9708, #13417, #12699, .T. ) ;
#13145 = CARTESIAN_POINT ( 'NONE',  ( 54.66261616134040935, 77.82294148670094103, -10.34700014260098477 ) ) ;
#13147 = VERTEX_POINT ( 'NONE', #20831 ) ;
#13148 = DIRECTION ( 'NONE',  ( -0.8660254037844354880, -0.5000000000000055511, 0.000000000000000000 ) ) ;
#13149 = CARTESIAN_POINT ( 'NONE',  ( 189.0671929290500088, 15.19036466668641872, -9.718744748712971671 ) ) ;
#13150 = ADVANCED_FACE ( 'NONE', ( #4631 ), #4853, .T. ) ;
#13151 = ORIENTED_EDGE ( 'NONE', *, *, #2027, .F. ) ;
#13152 = DIRECTION ( 'NONE',  ( -4.385380947269368335E-15, 1.000000000000000000, 0.000000000000000000 ) ) ;
#13153 = ORIENTED_EDGE ( 'NONE', *, *, #13762, .T. ) ;
#13154 = EDGE_CURVE ( 'NONE', #10151, #4077, #14617, .T. ) ;
#13155 = CARTESIAN_POINT ( 'NONE',  ( -30.20082347186430027, 65.74999999999995737, 2.745993778453658773 ) ) ;
#13156 = VERTEX_POINT ( 'NONE', #8213 ) ;
#13157 = DIRECTION ( 'NONE',  ( 0.8660254037844371533, 0.5000000000000026645, -6.661338147750938256E-16 ) ) ;
#13158 = CARTESIAN_POINT ( 'NONE',  ( 205.2117758015800462, 9.241723024529527208, -1.545471579934808215 ) ) ;
#13159 = EDGE_CURVE ( 'NONE', #18887, #8757, #6980, .T. ) ;
#13160 = LINE ( 'NONE', #19604, #17118 ) ;
#13161 = CARTESIAN_POINT ( 'NONE',  ( 206.1888006519934891, 10.33685784671313002, -25.96516918080908454 ) ) ;
#13162 = B_SPLINE_CURVE_WITH_KNOTS ( 'NONE', 3,
 ( #7679, #9262, #10978, #12470 ),
 .UNSPECIFIED., .F., .F.,
 ( 4, 4 ),
 ( 4.097547176954192966E-05, 0.0008949612097532494903 ),
 .UNSPECIFIED. ) ;
#13163 = ORIENTED_EDGE ( 'NONE', *, *, #977, .F. ) ;
#13164 = LINE ( 'NONE', #9851, #3732 ) ;
#13165 = DIRECTION ( 'NONE',  ( 1.000000000000000000, 0.000000000000000000, 0.000000000000000000 ) ) ;
#13166 = DIRECTION ( 'NONE',  ( -0.7071067811865462405, 8.659560562354950115E-17, -0.7071067811865489050 ) ) ;
#13167 = CIRCLE ( 'NONE', #6704, 5.999999999999989342 ) ;
#13168 = ORIENTED_EDGE ( 'NONE', *, *, #2573, .T. ) ;
#13170 = EDGE_CURVE ( 'NONE', #8072, #2271, #10770, .T. ) ;
#13169 = CARTESIAN_POINT ( 'NONE',  ( 5.000000000000004441, -2.342598717236899830, 4.057500000000059615 ) ) ;
#13171 = ORIENTED_EDGE ( 'NONE', *, *, #16022, .T. ) ;
#13172 = CARTESIAN_POINT ( 'NONE',  ( 81.75707366940763166, 56.44708661917523074, -1.582674401186259239 ) ) ;
#13173 = DIRECTION ( 'NONE',  ( 0.000000000000000000, -6.938893903907176763E-18, -1.000000000000000000 ) ) ;
#13174 = CARTESIAN_POINT ( 'NONE',  ( 79.54042647876013916, 49.99209421428520272, -9.220066387385379869 ) ) ;
#13175 = VERTEX_POINT ( 'NONE', #18089 ) ;
#13176 = ORIENTED_EDGE ( 'NONE', *, *, #861, .F. ) ;
#13177 = EDGE_LOOP ( 'NONE', ( #679, #14477, #8309, #13257, #20772, #6627, #8361, #8835, #944, #13854, #1427, #12867, #18805, #2288, #13674, #18432, #6239, #6143, #12027, #18840, #2879, #15068, #10727, #1154, #19124, #18049, #19550, #6284, #14170, #7672, #401, #14139, #3568, #13144, #10574, #16670, #840, #20694, #16456, #11402, #20326, #1596, #15403, #3157, #13253, #11111, #19622, #18623 ) ) ;
#13178 = ADVANCED_FACE ( 'NONE', ( #10108 ), #13215, .T. ) ;
#13179 = UNCERTAINTY_MEASURE_WITH_UNIT (LENGTH_MEASURE( 1.000000000000000082E-05 ), #4291, 'distance_accuracy_value', 'NONE');
#13180 = EDGE_CURVE ( 'NONE', #16971, #14800, #17391, .T. ) ;
#13181 = CARTESIAN_POINT ( 'NONE',  ( 172.3972143829816162, 19.35563505625646030, -14.00000000000000533 ) ) ;
#13182 = AXIS2_PLACEMENT_3D ( 'NONE', #14427, #3170, #9621 ) ;
#13183 = EDGE_LOOP ( 'NONE', ( #6955, #9643, #7170, #17233 ) ) ;
#13184 = DIRECTION ( 'NONE',  ( -0.4999999999999995004, 0.8660254037844390407, 0.000000000000000000 ) ) ;
#13185 = CARTESIAN_POINT ( 'NONE',  ( -28.35458678079950445, 80.00000000007563017, -1.908121642414536856 ) ) ;
#13186 = DIRECTION ( 'NONE',  ( 0.5000000000000007772, -0.8660254037844381525, 0.000000000000000000 ) ) ;
#13187 = CARTESIAN_POINT ( 'NONE',  ( 219.1036532380573192, 37.34809784919840325, -17.20332536629370068 ) ) ;
#13188 = EDGE_CURVE ( 'NONE', #10411, #16948, #16293, .T. ) ;
#13189 = VERTEX_POINT ( 'NONE', #274 ) ;
#13190 = EDGE_CURVE ( 'NONE', #9995, #10584, #1769, .T. ) ;
#13191 = DIRECTION ( 'NONE',  ( -0.5000000000000042188, 0.8660254037844361541, 1.401122807519728636E-16 ) ) ;
#13192 = EDGE_CURVE ( 'NONE', #19576, #13251, #6202, .T. ) ;
#13193 = CARTESIAN_POINT ( 'NONE',  ( 59.95697519919451679, 75.56535091951175787, -20.09837848646736802 ) ) ;
#13194 = CARTESIAN_POINT ( 'NONE',  ( -28.95046476526206192, 64.25000000000000000, 3.381771649840967342 ) ) ;
#13195 = ORIENTED_EDGE ( 'NONE', *, *, #6043, .T. ) ;
#13197 = EDGE_CURVE ( 'NONE', #1744, #16111, #17989, .T. ) ;
#13196 = DIRECTION ( 'NONE',  ( 0.8660254037844374864, 0.5000000000000021094, 6.938893903907228378E-16 ) ) ;
#13198 = CARTESIAN_POINT ( 'NONE',  ( 221.0616351780288653, 31.82541889109742073, -14.53509620734056540 ) ) ;
#13199 = VECTOR ( 'NONE', #3580, 1000.000000000000000 ) ;
#13200 = ORIENTED_EDGE ( 'NONE', *, *, #1389, .F. ) ;
#13201 = DIRECTION ( 'NONE',  ( 0.8660254037844370423, 0.5000000000000026645, -0.000000000000000000 ) ) ;
#13202 = ORIENTED_EDGE ( 'NONE', *, *, #16480, .F. ) ;
#13203 = DIRECTION ( 'NONE',  ( 0.7739085681710397013, 0.4468163201617135760, 0.4487991802004502873 ) ) ;
#13204 = DIRECTION ( 'NONE',  ( -0.8660254037844355990, -0.5000000000000055511, 0.000000000000000000 ) ) ;
#13205 = CARTESIAN_POINT ( 'NONE',  ( 216.7433590455158878, 9.780347600644502037, -22.03054070023868860 ) ) ;
#13206 = EDGE_CURVE ( 'NONE', #2569, #12601, #11643, .T. ) ;
#13207 = CARTESIAN_POINT ( 'NONE',  ( -15.00000000000000000, 0.000000000000000000, 28.99999999999999645 ) ) ;
#13208 = CARTESIAN_POINT ( 'NONE',  ( 215.5759555690916045, 8.333526798634666832, -24.58554911381534325 ) ) ;
#13209 = CARTESIAN_POINT ( 'NONE',  ( -28.99999999999999289, 0.000000000000000000, 15.00000000000000178 ) ) ;
#13210 = ORIENTED_EDGE ( 'NONE', *, *, #5523, .F. ) ;
#13211 = LINE ( 'NONE', #5231, #12523 ) ;
#13212 = ORIENTED_EDGE ( 'NONE', *, *, #4998, .F. ) ;
#13213 = LINE ( 'NONE', #17886, #17703 ) ;
#13214 = CARTESIAN_POINT ( 'NONE',  ( -3.815209910797584314, 53.56373870034735063, 2.796190595711027793 ) ) ;
#13215 = PLANE ( 'NONE',  #20089 ) ;
#13216 = DIRECTION ( 'NONE',  ( -0.5000000000000008882, 0.8660254037844381525, 0.000000000000000000 ) ) ;
#13217 = CARTESIAN_POINT ( 'NONE',  ( 709.3577481411962253, -862.5451554485315455, -14.00000000000005507 ) ) ;
#13218 = DIRECTION ( 'NONE',  ( -1.000000000000000000, -0.000000000000000000, -0.000000000000000000 ) ) ;
#13219 = EDGE_CURVE ( 'NONE', #6749, #7840, #11288, .T. ) ;
#13221 = ORIENTED_EDGE ( 'NONE', *, *, #9485, .F. ) ;
#13220 = VERTEX_POINT ( 'NONE', #8746 ) ;
#13222 = ORIENTED_EDGE ( 'NONE', *, *, #20161, .T. ) ;
#13223 = VERTEX_POINT ( 'NONE', #9127 ) ;
#13224 = CARTESIAN_POINT ( 'NONE',  ( 22.00490953756706958, 255.8427481158984165, -28.99999999999997513 ) ) ;
#13225 = LINE ( 'NONE', #17783, #2743 ) ;
#13226 = AXIS2_PLACEMENT_3D ( 'NONE', #11265, #13846, #17735 ) ;
#13227 = CIRCLE ( 'NONE', #7790, 11.50000000000002665 ) ;
#13228 = ORIENTED_EDGE ( 'NONE', *, *, #20111, .F. ) ;
#13229 = ORIENTED_EDGE ( 'NONE', *, *, #11349, .T. ) ;
#13230 = CARTESIAN_POINT ( 'NONE',  ( 226.8112919247088541, 41.21376214726366527, -10.60379488450932151 ) ) ;
#13231 = CARTESIAN_POINT ( 'NONE',  ( 226.9050879219818171, 41.70426184694306215, -11.10922658182122902 ) ) ;
#13232 = CARTESIAN_POINT ( 'NONE',  ( 229.5249483133369779, 36.84006146441270602, -12.55661888456621256 ) ) ;
#13233 = CARTESIAN_POINT ( 'NONE',  ( -12.32033641378040834, 60.86279337894578134, -3.389612121674974610 ) ) ;
#13234 = ORIENTED_EDGE ( 'NONE', *, *, #210, .T. ) ;
#13235 = VERTEX_POINT ( 'NONE', #18903 ) ;
#13236 = CARTESIAN_POINT ( 'NONE',  ( 84.01452848080118940, 118.4389375482329001, 4.000000000000000000 ) ) ;
#13237 = CIRCLE ( 'NONE', #4086, 3.902363844300875240 ) ;
#13238 = ORIENTED_EDGE ( 'NONE', *, *, #7291, .T. ) ;
#13239 = CARTESIAN_POINT ( 'NONE',  ( 216.1228831263525194, 15.89529313325283688, -12.59311507502024163 ) ) ;
#13240 = AXIS2_PLACEMENT_3D ( 'NONE', #5444, #14924, #389 ) ;
#13241 = AXIS2_PLACEMENT_3D ( 'NONE', #10941, #2787, #9228 ) ;
#13242 = CARTESIAN_POINT ( 'NONE',  ( 208.0983737146324870, 5.661548828456886895, -14.00000000000005507 ) ) ;
#13243 = CARTESIAN_POINT ( 'NONE',  ( -33.34256115809776588, 52.05794329512087160, -4.908380826879679582 ) ) ;
#13244 = CARTESIAN_POINT ( 'NONE',  ( -18.51262115207460823, 19.42532919514705370, 12.24574540514312204 ) ) ;
#13245 = VECTOR ( 'NONE', #20329, 1000.000000000000227 ) ;
#13246 = B_SPLINE_CURVE_WITH_KNOTS ( 'NONE', 3,
 ( #11005, #9604, #16100, #5899 ),
 .UNSPECIFIED., .F., .F.,
 ( 4, 4 ),
 ( 5.484421174515580465E-05, 0.0009088299497278719708 ),
 .UNSPECIFIED. ) ;
#13247 = DIRECTION ( 'NONE',  ( 0.000000000000000000, 0.000000000000000000, -1.000000000000000000 ) ) ;
#13248 = VECTOR ( 'NONE', #10438, 1000.000000000000227 ) ;
#13249 = CARTESIAN_POINT ( 'NONE',  ( 87.00490953756771262, 143.2594456239216925, 21.00000000000000711 ) ) ;
#13250 = EDGE_CURVE ( 'NONE', #5859, #3323, #12990, .T. ) ;
#13251 = VERTEX_POINT ( 'NONE', #13926 ) ;
#13252 = CARTESIAN_POINT ( 'NONE',  ( 56.88554678750333693, 76.87726758071406152, -7.198550218680361823 ) ) ;
#13253 = ORIENTED_EDGE ( 'NONE', *, *, #16488, .T. ) ;
#13254 = CARTESIAN_POINT ( 'NONE',  ( -3.332456710801453337, 66.65723886914538809, 2.419320319694736376 ) ) ;
#13255 = CARTESIAN_POINT ( 'NONE',  ( 229.0697140213455043, 37.95501946345524402, -17.20332536629375753 ) ) ;
#13256 = VECTOR ( 'NONE', #6088, 1000.000000000000000 ) ;
#13257 = ORIENTED_EDGE ( 'NONE', *, *, #7656, .T. ) ;
#13258 = DIRECTION ( 'NONE',  ( 0.5000000000000052180, -0.8660254037844355990, -0.000000000000000000 ) ) ;
#13259 = ADVANCED_FACE ( 'NONE', ( #5443, #10946 ), #20580, .F. ) ;
#13260 = CIRCLE ( 'NONE', #1418, 4.000000000000000000 ) ;
#13261 = CARTESIAN_POINT ( 'NONE',  ( -31.82323003959540486, 65.74999999999997158, 2.481238266578629226 ) ) ;
#13262 = ORIENTED_EDGE ( 'NONE', *, *, #6924, .F. ) ;
#13263 = LINE ( 'NONE', #8470, #10791 ) ;
#13264 = CARTESIAN_POINT ( 'NONE',  ( 214.9166615741016244, 8.725703323795450217, -24.01557619556987078 ) ) ;
#13265 = ORIENTED_EDGE ( 'NONE', *, *, #18627, .T. ) ;
#13266 = DIRECTION ( 'NONE',  ( 0.8660254037844380415, 0.5000000000000014433, 0.000000000000000000 ) ) ;
#13267 = CARTESIAN_POINT ( 'NONE',  ( 201.2663852398743529, 7.494899983462938842, -14.00000000000005507 ) ) ;
#13268 = EDGE_CURVE ( 'NONE', #18827, #20929, #17415, .T. ) ;
#13269 = ORIENTED_EDGE ( 'NONE', *, *, #18939, .F. ) ;
#13270 = CARTESIAN_POINT ( 'NONE',  ( 227.5312376355471145, 39.64027283883993391, -14.00000000000005507 ) ) ;
#13271 = PLANE ( 'NONE',  #15726 ) ;
#13272 = CARTESIAN_POINT ( 'NONE',  ( 197.7473131227538659, -1.187024626400782656, -12.53629070788332989 ) ) ;
#13273 = EDGE_CURVE ( 'NONE', #3253, #20919, #17728, .T. ) ;
#13274 = VERTEX_POINT ( 'NONE', #11942 ) ;
#13275 = DIRECTION ( 'NONE',  ( 0.000000000000000000, -1.000000000000000000, 6.938893903907177533E-18 ) ) ;
#13276 = PLANE ( 'NONE',  #8473 ) ;
#13277 = AXIS2_PLACEMENT_3D ( 'NONE', #7303, #2449, #18560 ) ;
#13278 = CARTESIAN_POINT ( 'NONE',  ( -12.32004792737159882, 69.13648218375620047, -3.389291572743964753 ) ) ;
#13279 = CARTESIAN_POINT ( 'NONE',  ( 79.37883709688843226, 49.55007393176662589, -13.67411419991173283 ) ) ;
#13281 = ORIENTED_EDGE ( 'NONE', *, *, #11445, .F. ) ;
#13280 = ORIENTED_EDGE ( 'NONE', *, *, #17202, .F. ) ;
#13282 = EDGE_CURVE ( 'NONE', #5897, #2748, #596, .T. ) ;
#13283 = ORIENTED_EDGE ( 'NONE', *, *, #20908, .T. ) ;
#13284 = ORIENTED_EDGE ( 'NONE', *, *, #589, .T. ) ;
#13285 = DIRECTION ( 'NONE',  ( 0.5547001962252345875, 0.000000000000000000, 0.8320502943378400573 ) ) ;
#13286 = ORIENTED_EDGE ( 'NONE', *, *, #8874, .F. ) ;
#13287 = CARTESIAN_POINT ( 'NONE',  ( 78.58128847415450480, 56.84536754178166262, -22.64245902371946784 ) ) ;
#13288 = CARTESIAN_POINT ( 'NONE',  ( -16.52214153618450254, 80.00000165566777355, -12.49590370130044903 ) ) ;
#13289 = CONICAL_SURFACE ( 'NONE', #11605, 10.85470691220533190, 0.8171114040043576665 ) ;
#13290 = CARTESIAN_POINT ( 'NONE',  ( -15.00000000000000000, -10.00000000000000000, 28.99999999999999645 ) ) ;
#13291 = CARTESIAN_POINT ( 'NONE',  ( 221.1038914607097183, 33.88358362032316506, -10.52303454827242213 ) ) ;
#13292 = EDGE_CURVE ( 'NONE', #19987, #5282, #18402, .T. ) ;
#13293 = ORIENTED_EDGE ( 'NONE', *, *, #19246, .T. ) ;
#13294 = VECTOR ( 'NONE', #11236, 1000.000000000000000 ) ;
#13295 = PLANE ( 'NONE',  #14660 ) ;
#13296 = ADVANCED_FACE ( 'NONE', ( #15736 ), #17521, .T. ) ;
#13297 = CARTESIAN_POINT ( 'NONE',  ( 77.09271508488680524, 67.80735157681689884, 0.1955130872258976915 ) ) ;
#13298 = CARTESIAN_POINT ( 'NONE',  ( 4.000000000000000000, -1.759474945355379072, 3.047500000000001652 ) ) ;
#13299 = PRODUCT_DEFINITION_SHAPE ( 'NONE', 'NONE',  #3795 ) ;
#13300 = VERTEX_POINT ( 'NONE', #10322 ) ;
#13301 = DIRECTION ( 'NONE',  ( 0.000000000000000000, 0.000000000000000000, 1.000000000000000000 ) ) ;
#13302 = FACE_OUTER_BOUND ( 'NONE', #4397, .T. ) ;
#13303 = DIRECTION ( 'NONE',  ( 0.5000000000000049960, -0.8660254037844358210, 0.000000000000000000 ) ) ;
#13304 = CARTESIAN_POINT ( 'NONE',  ( -13.92996325007571379, 79.99999999999890576, -12.33825502280066111 ) ) ;
#13305 = AXIS2_PLACEMENT_3D ( 'NONE', #8800, #16970, #12517 ) ;
#13306 = EDGE_CURVE ( 'NONE', #2200, #5521, #11533, .T. ) ;
#13308 = ORIENTED_EDGE ( 'NONE', *, *, #5319, .F. ) ;
#13307 = EDGE_LOOP ( 'NONE', ( #19621, #7930, #736, #13356 ) ) ;
#13309 = EDGE_CURVE ( 'NONE', #5971, #7973, #7884, .T. ) ;
#13310 = DIRECTION ( 'NONE',  ( 0.000000000000000000, 0.000000000000000000, -1.000000000000000000 ) ) ;
#13311 = CARTESIAN_POINT ( 'NONE',  ( 208.8107687779841228, 4.427644383670616079, -14.00000000000005507 ) ) ;
#13312 = DIRECTION ( 'NONE',  ( -0.8660254037844380415, -0.5000000000000014433, -0.000000000000000000 ) ) ;
#13313 = CARTESIAN_POINT ( 'NONE',  ( 226.6211368133091923, 39.11482588413117867, -14.00000000000005507 ) ) ;
#13314 = CARTESIAN_POINT ( 'NONE',  ( -30.00000000000040146, 4.999999999999647393, -3.756581053969355821 ) ) ;
#13315 = DIRECTION ( 'NONE',  ( 0.5000000000000051070, -0.8660254037844359321, 0.000000000000000000 ) ) ;
#13316 = EDGE_CURVE ( 'NONE', #19592, #19576, #20394, .T. ) ;
#13317 = ORIENTED_EDGE ( 'NONE', *, *, #18738, .T. ) ;
#13318 = CARTESIAN_POINT ( 'NONE',  ( 80.02873681804580031, 56.10702248625631228, -22.01643817346699450 ) ) ;
#13319 = LINE ( 'NONE', #11506, #15240 ) ;
#13320 = AXIS2_PLACEMENT_3D ( 'NONE', #9751, #8055, #1820 ) ;
#13321 = VERTEX_POINT ( 'NONE', #14146 ) ;
#13322 = CARTESIAN_POINT ( 'NONE',  ( 221.0683110530012527, 31.81385593646023935, -13.56204498775467115 ) ) ;
#13323 = CARTESIAN_POINT ( 'NONE',  ( 1.287529140580364606, 55.27775868348017241, -1.071617489983800908 ) ) ;
#13324 = CARTESIAN_POINT ( 'NONE',  ( -0.1082929358729399077, 78.60836521392512566, -6.178814694513294015 ) ) ;
#13325 = ADVANCED_FACE ( 'NONE', ( #7432 ), #19980, .F. ) ;
#13326 = DIRECTION ( 'NONE',  ( -0.5000000000000039968, 0.8660254037844363761, 0.000000000000000000 ) ) ;
#13327 = CARTESIAN_POINT ( 'NONE',  ( 42.30949999999999989, 0.000000000000000000, 3.999999999999999112 ) ) ;
#13328 = CARTESIAN_POINT ( 'NONE',  ( 221.8919835788506987, 32.51856803065840040, -16.00491213559322290 ) ) ;
#13330 = ORIENTED_EDGE ( 'NONE', *, *, #10126, .T. ) ;
#13329 = ORIENTED_EDGE ( 'NONE', *, *, #19317, .F. ) ;
#13331 = ORIENTED_EDGE ( 'NONE', *, *, #20883, .F. ) ;
#13332 = CARTESIAN_POINT ( 'NONE',  ( 215.6983787324637376, 15.82721531135244675, -16.75125533358882279 ) ) ;
#13333 = CARTESIAN_POINT ( 'NONE',  ( 205.8534188064671469, 2.720217581527302642, -2.669358488461094581 ) ) ;
#13334 = EDGE_LOOP ( 'NONE', ( #9795, #19554, #2954, #8271 ) ) ;
#13335 = VERTEX_POINT ( 'NONE', #1197 ) ;
#13336 = SURFACE_SIDE_STYLE ('',( #15364 ) ) ;
#13337 = DIRECTION ( 'NONE',  ( 0.000000000000000000, 0.000000000000000000, -1.000000000000000000 ) ) ;
#13338 = LINE ( 'NONE', #17042, #17146 ) ;
#13339 = AXIS2_PLACEMENT_3D ( 'NONE', #445, #18455, #7103 ) ;
#13340 = EDGE_LOOP ( 'NONE', ( #11040, #6726, #13016, #20175, #1134 ) ) ;
#13341 = DIRECTION ( 'NONE',  ( 0.000000000000000000, -1.000000000000000000, 0.000000000000000000 ) ) ;
#13342 = DIRECTION ( 'NONE',  ( -0.8660254037844380415, -0.5000000000000014433, -0.000000000000000000 ) ) ;
#13343 = VERTEX_POINT ( 'NONE', #2998 ) ;
#13344 = CARTESIAN_POINT ( 'NONE',  ( 191.5478494775925640, 36.18576207517880050, -14.00000000000006395 ) ) ;
#13345 = B_SPLINE_CURVE_WITH_KNOTS ( 'NONE', 3,
 ( #5334, #14918, #4930, #6836 ),
 .UNSPECIFIED., .F., .F.,
 ( 4, 4 ),
 ( 3.206650225968376458E-07, 0.0004523739068024474762 ),
 .UNSPECIFIED. ) ;
#13346 = B_SPLINE_CURVE_WITH_KNOTS ( 'NONE', 3,
 ( #1379, #7832, #19388, #11436, #3, #1586, #11238, #14331, #14538, #4756, #20763, #12722, #15811, #3071, #19185, #6538, #16021, #14430, #6333, #9725 ),
 .UNSPECIFIED., .F., .F.,
 ( 4, 2, 2, 2, 2, 2, 2, 2, 2, 4 ),
 ( 0.09234794266491903880, 0.09522624378769738163, 0.09810454491047572445, 0.1038611471560324101, 0.1067394482788107390, 0.1096177494015890680, 0.1124960505243673969, 0.1139352010857565822, 0.1146547763664511471, 0.1153743516471457259 ),
 .UNSPECIFIED. ) ;
#13347 = DIRECTION ( 'NONE',  ( -0.8660254037844355990, -0.5000000000000054401, -7.092004947830981940E-15 ) ) ;
#13348 = CARTESIAN_POINT ( 'NONE',  ( -28.43641358195718283, 53.09495409546831013, -3.357527245236496594 ) ) ;
#13349 = CARTESIAN_POINT ( 'NONE',  ( 24.01452848080067071, 222.3619860023652564, 26.00000000000001776 ) ) ;
#13350 = EDGE_CURVE ( 'NONE', #14531, #16924, #4485, .T. ) ;
#13351 = CARTESIAN_POINT ( 'NONE',  ( 205.0042238655992719, 9.652942120212628652, -25.96516918080906677 ) ) ;
#13352 = CARTESIAN_POINT ( 'NONE',  ( 208.4761278624580711, 5.007259451653140125, -14.00000000000005507 ) ) ;
#13353 = ORIENTED_EDGE ( 'NONE', *, *, #6938, .T. ) ;
#13354 = ORIENTED_EDGE ( 'NONE', *, *, #3317, .T. ) ;
#13355 = CARTESIAN_POINT ( 'NONE',  ( 54.59993483903557632, 77.84956924708853876, -14.48805868377909611 ) ) ;
#13356 = ORIENTED_EDGE ( 'NONE', *, *, #4813, .F. ) ;
#13357 = ORIENTED_EDGE ( 'NONE', *, *, #195, .T. ) ;
#13358 = CARTESIAN_POINT ( 'NONE',  ( 210.5941221282246545, 5.457263920492195552, -2.233628351993232730 ) ) ;
#13359 = DIRECTION ( 'NONE',  ( 0.2300325188655826802, -0.3984280100682314751, -0.8878852184023702243 ) ) ;
#13360 = ORIENTED_EDGE ( 'NONE', *, *, #16276, .T. ) ;
#13361 = LINE ( 'NONE', #6553, #14817 ) ;
#13362 = AXIS2_PLACEMENT_3D ( 'NONE', #14584, #3121, #15959 ) ;
#13363 = FACE_OUTER_BOUND ( 'NONE', #5695, .T. ) ;
#13364 = ORIENTED_EDGE ( 'NONE', *, *, #1320, .F. ) ;
#13365 = EDGE_CURVE ( 'NONE', #12398, #18916, #5964, .T. ) ;
#13366 = CARTESIAN_POINT ( 'NONE',  ( 5.000000000000004441, 0.000000000000000000, 0.000000000000000000 ) ) ;
#13367 = CARTESIAN_POINT ( 'NONE',  ( 5.000000000000004441, 4.687458767389385798E-16, -4.057500000000029416 ) ) ;
#13368 = ORIENTED_EDGE ( 'NONE', *, *, #15494, .F. ) ;
#13369 = CARTESIAN_POINT ( 'NONE',  ( 157.3972143829815309, 45.33639716978957068, -22.00000000000007816 ) ) ;
#13370 = CARTESIAN_POINT ( 'NONE',  ( 213.4541640218532166, 5.845417697364395870, -14.00000000000005507 ) ) ;
#13371 = DIRECTION ( 'NONE',  ( -0.5000000000000049960, 0.8660254037844357100, -0.000000000000000000 ) ) ;
#13372 = CARTESIAN_POINT ( 'NONE',  ( 221.1519434606206005, 33.18250674572787062, -11.35524774226752598 ) ) ;
#13373 = DIRECTION ( 'NONE',  ( -0.5000000000000041078, 0.8660254037844363761, 0.000000000000000000 ) ) ;
#13374 = ORIENTED_EDGE ( 'NONE', *, *, #12686, .F. ) ;
#13375 = LINE ( 'NONE', #6572, #715 ) ;
#13376 = CARTESIAN_POINT ( 'NONE',  ( 201.8424605768971389, 26.45147170171050277, -13.51420023870525711 ) ) ;
#13377 = LINE ( 'NONE', #8272, #12190 ) ;
#13378 = CARTESIAN_POINT ( 'NONE',  ( 79.36280640676876885, 49.50636784572148485, -13.14917256677527746 ) ) ;
#13380 = VERTEX_POINT ( 'NONE', #19113 ) ;
#13379 = VERTEX_POINT ( 'NONE', #1100 ) ;
#13381 = B_SPLINE_CURVE_WITH_KNOTS ( 'NONE', 3,
 ( #20790, #11152, #16052, #1513 ),
 .UNSPECIFIED., .F., .F.,
 ( 4, 4 ),
 ( 2.916652381017237348E-07, 0.0006729424572952378593 ),
 .UNSPECIFIED. ) ;
#13382 = ORIENTED_EDGE ( 'NONE', *, *, #2171, .T. ) ;
#13383 = ADVANCED_FACE ( 'NONE', ( #4585 ), #11052, .T. ) ;
#13384 = B_SPLINE_CURVE_WITH_KNOTS ( 'NONE', 3,
 ( #12772, #1842, #9571, #8284 ),
 .UNSPECIFIED., .F., .F.,
 ( 4, 4 ),
 ( 4.751027867067633455E-07, 0.0004525283445666252878 ),
 .UNSPECIFIED. ) ;
#13385 = CARTESIAN_POINT ( 'NONE',  ( 216.2725394319739110, 15.91768827161142674, -14.00000000000005507 ) ) ;
#13386 = ORIENTED_EDGE ( 'NONE', *, *, #14603, .T. ) ;
#13387 = DIRECTION ( 'NONE',  ( 0.8660254037844370423, 0.5000000000000026645, -0.000000000000000000 ) ) ;
#13388 = EDGE_CURVE ( 'NONE', #13569, #2452, #4788, .T. ) ;
#13389 = CIRCLE ( 'NONE', #14772, 4.999999999999990230 ) ;
#13390 = CYLINDRICAL_SURFACE ( 'NONE', #17220, 12.47473710546057646 ) ;
#13391 = CARTESIAN_POINT ( 'NONE',  ( -15.00000000000000000, 0.000000000000000000, 28.99999999999999645 ) ) ;
#13392 = CARTESIAN_POINT ( 'NONE',  ( 196.2730226335446844, 4.434970834353566538, -8.544894389632862186 ) ) ;
#13393 = ORIENTED_EDGE ( 'NONE', *, *, #13794, .F. ) ;
#13394 = CARTESIAN_POINT ( 'NONE',  ( -15.99999999999999289, 64.25000000000000000, 4.999999999999989342 ) ) ;
#13395 = CIRCLE ( 'NONE', #13067, 1.499999999999993783 ) ;
#13396 = EDGE_CURVE ( 'NONE', #11673, #20270, #16088, .T. ) ;
#13397 = CARTESIAN_POINT ( 'NONE',  ( 60.75500010343246515, 75.22326679826591089, -20.54849183009933711 ) ) ;
#13398 = LINE ( 'NONE', #5115, #1967 ) ;
#13399 = ORIENTED_EDGE ( 'NONE', *, *, #16651, .T. ) ;
#13400 =( REPRESENTATION_RELATIONSHIP ('NONE','NONE', #4634, #6230 ) REPRESENTATION_RELATIONSHIP_WITH_TRANSFORMATION ( #19706 )SHAPE_REPRESENTATION_RELATIONSHIP( ) );
#13401 = DIRECTION ( 'NONE',  ( 0.8601696498176548689, 0.4966191788709768407, -0.1160929141252376451 ) ) ;
#13402 = CARTESIAN_POINT ( 'NONE',  ( 217.9247606104526085, 37.25864501911015481, -16.29291827778580526 ) ) ;
#13403 = CARTESIAN_POINT ( 'NONE',  ( 205.8264633344831225, 9.596613037118636669, -14.00000000000005507 ) ) ;
#13404 = CARTESIAN_POINT ( 'NONE',  ( -3.762162058313276436, 80.00000000009157475, -2.568690455533788164 ) ) ;
#13405 = EDGE_CURVE ( 'NONE', #13379, #17056, #1411, .T. ) ;
#13406 = ORIENTED_EDGE ( 'NONE', *, *, #17442, .F. ) ;
#13407 = AXIS2_PLACEMENT_3D ( 'NONE', #15391, #8987, #4015 ) ;
#13408 = FACE_OUTER_BOUND ( 'NONE', #16768, .T. ) ;
#13409 = DIRECTION ( 'NONE',  ( -0.8660254037844355990, -0.5000000000000055511, 0.000000000000000000 ) ) ;
#13410 = CIRCLE ( 'NONE', #11051, 12.00000000000002665 ) ;
#13411 = CARTESIAN_POINT ( 'NONE',  ( -31.89200696759080600, 78.60820088387509941, -6.178462522043184357 ) ) ;
#13412 = ORIENTED_EDGE ( 'NONE', *, *, #10714, .T. ) ;
#13413 = EDGE_CURVE ( 'NONE', #17484, #2297, #3832, .T. ) ;
#13414 = CARTESIAN_POINT ( 'NONE',  ( 206.1888006519934891, 10.33685784671313002, -25.96516918080908454 ) ) ;
#13415 =( LENGTH_UNIT ( ) NAMED_UNIT ( * ) SI_UNIT ( .MILLI., .METRE. ) );
#13416 = CARTESIAN_POINT ( 'NONE',  ( 226.1375891942321061, 43.03360863815010617, -16.20791459969590775 ) ) ;
#13417 = VERTEX_POINT ( 'NONE', #6461 ) ;
#13418 = CARTESIAN_POINT ( 'NONE',  ( 80.59332237824474987, 57.28794717993011432, -22.99282313644232900 ) ) ;
#13419 = EDGE_CURVE ( 'NONE', #3051, #951, #12663, .T. ) ;
#13420 = VECTOR ( 'NONE', #3833, 1000.000000000000000 ) ;
#13421 = CARTESIAN_POINT ( 'NONE',  ( -3.502006981982628719, 48.75774031421161681, -0.5664283305349653297 ) ) ;
#13422 = EDGE_CURVE ( 'NONE', #9110, #18065, #19731, .T. ) ;
#13423 = ORIENTED_EDGE ( 'NONE', *, *, #12001, .T. ) ;
#13424 = AXIS2_PLACEMENT_3D ( 'NONE', #11957, #716, #5781 ) ;
#13425 = CARTESIAN_POINT ( 'NONE',  ( 201.8234976231972553, 26.52995303002161265, -14.09970077338581973 ) ) ;
#13426 = CARTESIAN_POINT ( 'NONE',  ( -3.160111173998752854, 59.48252478531676957, 1.461028833307322694 ) ) ;
#13427 = CARTESIAN_POINT ( 'NONE',  ( 212.8611117457045907, 7.023710210201398851, -25.12838443884023576 ) ) ;
#13428 = AXIS2_PLACEMENT_3D ( 'NONE', #7050, #19559, #10221 ) ;
#13429 = CARTESIAN_POINT ( 'NONE',  ( 0.000000000000000000, 8.878689293818310074E-16, -6.500000000000000888 ) ) ;
#13430 = CARTESIAN_POINT ( 'NONE',  ( 97.12292291349348261, 198.8252231143156621, 9.741427369672765124 ) ) ;
#13431 = B_SPLINE_CURVE_WITH_KNOTS ( 'NONE', 3,
 ( #265, #19549, #14607, #1965 ),
 .UNSPECIFIED., .F., .F.,
 ( 4, 4 ),
 ( 4.029077177025402201E-07, 0.0005663291300164543813 ),
 .UNSPECIFIED. ) ;
#13432 = FACE_OUTER_BOUND ( 'NONE', #3537, .T. ) ;
#13434 = ORIENTED_EDGE ( 'NONE', *, *, #13776, .F. ) ;
#13433 = ORIENTED_EDGE ( 'NONE', *, *, #13146, .T. ) ;
#13435 = VERTEX_POINT ( 'NONE', #11360 ) ;
#13436 = CARTESIAN_POINT ( 'NONE',  ( 27.33329038210763784, 64.25000000000000000, -2.193932927905873687 ) ) ;
#13437 = CARTESIAN_POINT ( 'NONE',  ( -35.00000000000000000, 65.00000000000000000, -12.50000000000000000 ) ) ;
#13438 = ADVANCED_FACE ( 'NONE', ( #11462 ), #20419, .F. ) ;
#13439 = EDGE_LOOP ( 'NONE', ( #16636, #14211, #2226, #10353 ) ) ;
#13440 = DIRECTION ( 'NONE',  ( -0.5000000000000008882, 0.8660254037844381525, 0.000000000000000000 ) ) ;
#13441 = CARTESIAN_POINT ( 'NONE',  ( 227.8578996646062933, 40.05394349866928394, -17.56803216753788988 ) ) ;
#13442 = FACE_OUTER_BOUND ( 'NONE', #3062, .T. ) ;
#13443 = ORIENTED_EDGE ( 'NONE', *, *, #17442, .T. ) ;
#13444 = DIRECTION ( 'NONE',  ( 0.6634139481689433904, 0.3830222215594973889, 0.6427876096865291489 ) ) ;
#13445 = VECTOR ( 'NONE', #17818, 1000.000000000000000 ) ;
#13446 = LINE ( 'NONE', #16831, #20217 ) ;
#13447 = EDGE_CURVE ( 'NONE', #305, #10186, #9852, .T. ) ;
#13448 = VERTEX_POINT ( 'NONE', #17626 ) ;
#13449 = CARTESIAN_POINT ( 'NONE',  ( 219.9079348888217567, 10.83459622500478048, -11.01983352639526714 ) ) ;
#13450 = ADVANCED_FACE ( 'NONE', ( #11150 ), #16237, .T. ) ;
#13451 = CARTESIAN_POINT ( 'NONE',  ( 208.4761278624580711, 5.007259451653140125, -14.00000000000005507 ) ) ;
#13452 = CARTESIAN_POINT ( 'NONE',  ( -27.70464211192128445, 45.99281090038124375, -4.438302275953727616 ) ) ;
#13453 = CARTESIAN_POINT ( 'NONE',  ( 212.8527399996651752, 6.761277556564890823, -3.125199447383528284 ) ) ;
#13454 = ORIENTED_EDGE ( 'NONE', *, *, #9955, .F. ) ;
#13455 = DIRECTION ( 'NONE',  ( 0.000000000000000000, 0.000000000000000000, -1.000000000000000000 ) ) ;
#13456 = DIRECTION ( 'NONE',  ( -0.7951984747223579397, -0.4591080534401397184, 0.3960797660391670583 ) ) ;
#13457 = AXIS2_PLACEMENT_3D ( 'NONE', #8442, #11531, #11429 ) ;
#13459 = ORIENTED_EDGE ( 'NONE', *, *, #12033, .F. ) ;
#13458 = ORIENTED_EDGE ( 'NONE', *, *, #2575, .F. ) ;
#13460 = CARTESIAN_POINT ( 'NONE',  ( 56.17290541411050953, 77.18071550550122595, -17.04775252395419116 ) ) ;
#13461 = CIRCLE ( 'NONE', #12453, 16.50000000000000000 ) ;
#13462 = ORIENTED_EDGE ( 'NONE', *, *, #19568, .T. ) ;
#13463 = ORIENTED_EDGE ( 'NONE', *, *, #6551, .F. ) ;
#13464 = CARTESIAN_POINT ( 'NONE',  ( 218.5272241891094325, 10.03744253085286964, -18.09983247376310089 ) ) ;
#13465 = DIRECTION ( 'NONE',  ( -0.7499999999999953371, -0.4330127018922228510, 0.5000000000000038858 ) ) ;
#13466 = B_SPLINE_CURVE_WITH_KNOTS ( 'NONE', 3,
 ( #15598, #14329, #10693, #9206 ),
 .UNSPECIFIED., .F., .F.,
 ( 4, 4 ),
 ( 5.145664760488188064E-07, 0.0005664407887627788104 ),
 .UNSPECIFIED. ) ;
#13467 = ORIENTED_EDGE ( 'NONE', *, *, #15780, .T. ) ;
#13468 = CARTESIAN_POINT ( 'NONE',  ( 220.3379489458267528, 34.59238660243320851, -17.48830818005197330 ) ) ;
#13469 = CARTESIAN_POINT ( 'NONE',  ( 227.9553588074475670, 39.88513931160575510, -14.00000000000005507 ) ) ;
#13470 = VERTEX_POINT ( 'NONE', #14675 ) ;
#13471 = VECTOR ( 'NONE', #15262, 1000.000000000000114 ) ;
#13472 = PRODUCT_DEFINITION_SHAPE ( 'NONE', 'NONE',  #11582 ) ;
#13473 = DIRECTION ( 'NONE',  ( 0.000000000000000000, 0.000000000000000000, -1.000000000000000000 ) ) ;
#13474 = FACE_OUTER_BOUND ( 'NONE', #2328, .T. ) ;
#13475 = B_SPLINE_CURVE_WITH_KNOTS ( 'NONE', 3,
 ( #18126, #8466, #14970, #13468 ),
 .UNSPECIFIED., .F., .F.,
 ( 4, 4 ),
 ( 1.468788439215023033E-06, 0.0005869571441788198549 ),
 .UNSPECIFIED. ) ;
#13476 = AXIS2_PLACEMENT_3D ( 'NONE', #4053, #989, #2479 ) ;
#13477 = PLANE ( 'NONE',  #67 ) ;
#13478 = DIRECTION ( 'NONE',  ( -0.8660254037844355990, -0.5000000000000055511, 0.000000000000000000 ) ) ;
#13479 = DIRECTION ( 'NONE',  ( 0.000000000000000000, -1.000000000000000000, 0.000000000000000000 ) ) ;
#13480 = ORIENTED_EDGE ( 'NONE', *, *, #19079, .T. ) ;
#13481 = CARTESIAN_POINT ( 'NONE',  ( 203.1555906521724637, 1.162625770417896609, -2.579136038830115218 ) ) ;
#13482 = CARTESIAN_POINT ( 'NONE',  ( -15.99999999999998934, 4.999999999999997335, 17.50000000000000000 ) ) ;
#13483 = CARTESIAN_POINT ( 'NONE',  ( 207.3371157680689407, 10.99983788809380236, -1.383673999417951439 ) ) ;
#13484 = ORIENTED_EDGE ( 'NONE', *, *, #14119, .T. ) ;
#13485 = CARTESIAN_POINT ( 'NONE',  ( 80.72059958497800380, 57.56183285562485707, -1.811819122334661358 ) ) ;
#13486 = COLOUR_RGB ( '',0.7921568627450980005, 0.8196078431372548767, 0.9333333333333333481 ) ;
#13487 = EDGE_CURVE ( 'NONE', #14131, #17716, #1511, .T. ) ;
#13488 = LINE ( 'NONE', #7218, #9460 ) ;
#13489 = CARTESIAN_POINT ( 'NONE',  ( 80.42500778927126248, 52.45643482355421128, -4.799589912607079789 ) ) ;
#13490 = VECTOR ( 'NONE', #10688, 1000.000000000000114 ) ;
#13492 = ORIENTED_EDGE ( 'NONE', *, *, #11234, .F. ) ;
#13491 = ORIENTED_EDGE ( 'NONE', *, *, #11471, .T. ) ;
#13493 = APPLICATION_PROTOCOL_DEFINITION ( 'draft international standard', 'automotive_design', 1998, #20813 ) ;
#13494 = ORIENTED_EDGE ( 'NONE', *, *, #2278, .T. ) ;
#13495 = DIRECTION ( 'NONE',  ( 0.000000000000000000, 0.000000000000000000, 1.000000000000000000 ) ) ;
#13496 = ORIENTED_EDGE ( 'NONE', *, *, #12987, .F. ) ;
#13497 = CARTESIAN_POINT ( 'NONE',  ( 81.68143887139700610, 63.75701689938041739, -25.44160877821855848 ) ) ;
#13498 = CARTESIAN_POINT ( 'NONE',  ( -18.58414241182626014, 79.99915570207093651, -12.30640999581614103 ) ) ;
#13499 = CARTESIAN_POINT ( 'NONE',  ( 198.4028805101389992, 5.310605495132000975, -23.06309126349794170 ) ) ;
#13500 = DIRECTION ( 'NONE',  ( 1.000000000000000000, 0.000000000000000000, 0.000000000000000000 ) ) ;
#13501 = ORIENTED_EDGE ( 'NONE', *, *, #9899, .T. ) ;
#13502 = EDGE_CURVE ( 'NONE', #3214, #1853, #4985, .T. ) ;
#13503 = VECTOR ( 'NONE', #4368, 1000.000000000000227 ) ;
#13504 = CARTESIAN_POINT ( 'NONE',  ( 84.01452848080126046, 118.4389375482328859, 55.99999999999997868 ) ) ;
#13505 = CARTESIAN_POINT ( 'NONE',  ( -15.99999999999999289, 9.999999999999994671, 0.000000000000000000 ) ) ;
#13506 = LINE ( 'NONE', #8719, #18217 ) ;
#13507 = CARTESIAN_POINT ( 'NONE',  ( 199.2144802262915846, 21.04890371929339921, -14.00000000000005507 ) ) ;
#13508 = ADVANCED_FACE ( 'NONE', ( #7959 ), #6529, .T. ) ;
#13509 = FACE_OUTER_BOUND ( 'NONE', #4408, .T. ) ;
#13510 = ADVANCED_FACE ( 'NONE', ( #17736 ), #1145, .T. ) ;
#13511 = DIRECTION ( 'NONE',  ( 0.8660254037844360431, 0.5000000000000044409, 0.000000000000000000 ) ) ;
#13512 = CARTESIAN_POINT ( 'NONE',  ( -8.889222525793472940, 79.96752057144499304, -11.48167302094788589 ) ) ;
#13514 = ORIENTED_EDGE ( 'NONE', *, *, #19711, .T. ) ;
#13513 = EDGE_LOOP ( 'NONE', ( #1987, #19193, #18329, #20637 ) ) ;
#13515 = AXIS2_PLACEMENT_3D ( 'NONE', #8688, #16751, #5388 ) ;
#13516 = CARTESIAN_POINT ( 'NONE',  ( -15.99999999999999289, 64.25000000000000000, 0.000000000000000000 ) ) ;
#13517 = LINE ( 'NONE', #19963, #2775 ) ;
#13518 = DIRECTION ( 'NONE',  ( 0.000000000000000000, -1.000000000000000000, 0.000000000000000000 ) ) ;
#13519 = ORIENTED_EDGE ( 'NONE', *, *, #20501, .T. ) ;
#13520 = CARTESIAN_POINT ( 'NONE',  ( 77.44988535257863305, 70.55865560739972864, -25.18692877124620466 ) ) ;
#13521 = DIRECTION ( 'NONE',  ( -0.8660254037844355990, -0.5000000000000055511, 0.000000000000000000 ) ) ;
#13522 = ORIENTED_EDGE ( 'NONE', *, *, #6956, .T. ) ;
#13523 = CARTESIAN_POINT ( 'NONE',  ( 81.45340819612970051, 61.78983808953367429, -25.10003246456431825 ) ) ;
#13524 = FACE_OUTER_BOUND ( 'NONE', #14988, .T. ) ;
#13525 = APPLICATION_CONTEXT ( 'automotive_design' ) ;
#13526 = CIRCLE ( 'NONE', #1680, 11.98469917212512215 ) ;
#13527 = ORIENTED_EDGE ( 'NONE', *, *, #5586, .T. ) ;
#13528 = CARTESIAN_POINT ( 'NONE',  ( 4.000000000000000000, 3.518949890710767026, -4.987329993433320396E-15 ) ) ;
#13529 = CARTESIAN_POINT ( 'NONE',  ( -3.315871571232889448, 53.81292811603974258, -2.490183643791233692 ) ) ;
#13530 = DIRECTION ( 'NONE',  ( 0.000000000000000000, 0.000000000000000000, -1.000000000000000000 ) ) ;
#13531 = FACE_OUTER_BOUND ( 'NONE', #9948, .T. ) ;
#13532 = ADVANCED_FACE ( 'NONE', ( #17938 ), #9653, .F. ) ;
#13533 = CARTESIAN_POINT ( 'NONE',  ( 62.00490953756744972, 186.5607158131434744, 26.00000000000001776 ) ) ;
#13534 = CARTESIAN_POINT ( 'NONE',  ( 228.9655759139732538, 38.13539195642837143, -16.94731950718130520 ) ) ;
#13535 = ADVANCED_FACE ( 'NONE', ( #19610 ), #5088, .F. ) ;
#13537 = VERTEX_POINT ( 'NONE', #10060 ) ;
#13536 = ORIENTED_EDGE ( 'NONE', *, *, #3382, .F. ) ;
#13538 = ORIENTED_EDGE ( 'NONE', *, *, #4468, .T. ) ;
#13539 = CYLINDRICAL_SURFACE ( 'NONE', #4081, 12.47473710546057646 ) ;
#13540 = CARTESIAN_POINT ( 'NONE',  ( 4.000000000000000000, 3.518949890710767026, -4.987329993433320396E-15 ) ) ;
#13541 = AXIS2_PLACEMENT_3D ( 'NONE', #10954, #1311, #19318 ) ;
#13542 = ORIENTED_EDGE ( 'NONE', *, *, #15291, .F. ) ;
#13543 = EDGE_LOOP ( 'NONE', ( #19994, #18755, #5582, #5420 ) ) ;
#13544 = VERTEX_POINT ( 'NONE', #3609 ) ;
#13545 = CARTESIAN_POINT ( 'NONE',  ( 78.25962792613263730, 56.38842605307239353, -2.753243699805369982 ) ) ;
#13546 = CARTESIAN_POINT ( 'NONE',  ( 215.3856909933734300, 6.960585314318631589, -14.00000000000005329 ) ) ;
#13547 = DIRECTION ( 'NONE',  ( -0.5000000000000045519, 0.8660254037844360431, 0.000000000000000000 ) ) ;
#13548 = CIRCLE ( 'NONE', #6748, 11.94520687646042667 ) ;
#13549 = VERTEX_POINT ( 'NONE', #1929 ) ;
#13550 = AXIS2_PLACEMENT_3D ( 'NONE', #10392, #13500, #10289 ) ;
#13551 = EDGE_CURVE ( 'NONE', #3963, #2749, #8592, .T. ) ;
#13552 = DIRECTION ( 'NONE',  ( -0.5000000000000045519, 0.8660254037844361541, 0.000000000000000000 ) ) ;
#13553 = DIRECTION ( 'NONE',  ( -0.8660254037844360431, -0.5000000000000044409, 5.976026924694052093E-17 ) ) ;
#13554 = CIRCLE ( 'NONE', #680, 1.500000000000001332 ) ;
#13555 = CARTESIAN_POINT ( 'NONE',  ( 227.5262471203226085, 39.97542342332531007, -10.20315278194655662 ) ) ;
#13556 = EDGE_CURVE ( 'NONE', #18457, #15672, #16443, .T. ) ;
#13557 = DIRECTION ( 'NONE',  ( 0.8660254037844360431, 0.5000000000000045519, 0.000000000000000000 ) ) ;
#13558 = CARTESIAN_POINT ( 'NONE',  ( -25.95795895568129197, 50.50501676485125557, -7.579117145205284345 ) ) ;
#13559 = DIRECTION ( 'NONE',  ( -0.8660254037844354880, -0.5000000000000055511, 0.000000000000000000 ) ) ;
#13560 = EDGE_CURVE ( 'NONE', #7157, #12427, #10609, .T. ) ;
#13561 = CARTESIAN_POINT ( 'NONE',  ( 228.5767221322753073, 38.80890646304447955, -10.64970491435236077 ) ) ;
#13562 = DIRECTION ( 'NONE',  ( 0.4999999999999995004, -0.8660254037844390407, 0.000000000000000000 ) ) ;
#13564 = ORIENTED_EDGE ( 'NONE', *, *, #3394, .F. ) ;
#13563 = ORIENTED_EDGE ( 'NONE', *, *, #17768, .F. ) ;
#13565 = CARTESIAN_POINT ( 'NONE',  ( 62.88012315395636875, 78.01512619438163654, -12.57944489567368329 ) ) ;
#13566 = AXIS2_PLACEMENT_3D ( 'NONE', #3129, #11390, #11290 ) ;
#13567 = ORIENTED_EDGE ( 'NONE', *, *, #2684, .F. ) ;
#13568 = VERTEX_POINT ( 'NONE', #18353 ) ;
#13569 = VERTEX_POINT ( 'NONE', #2031 ) ;
#13570 = CARTESIAN_POINT ( 'NONE',  ( 207.8344881237125890, 4.636808575765666518, -26.45271578590683248 ) ) ;
#13571 = PLANE ( 'NONE',  #14109 ) ;
#13572 = VECTOR ( 'NONE', #20566, 1000.000000000000227 ) ;
#13573 = ADVANCED_FACE ( 'NONE', ( #15090 ), #20043, .F. ) ;
#13574 = ADVANCED_FACE ( 'NONE', ( #16549 ), #12329, .T. ) ;
#13575 = ORIENTED_EDGE ( 'NONE', *, *, #4409, .F. ) ;
#13576 = DIRECTION ( 'NONE',  ( 1.000000000000000000, -0.000000000000000000, -0.000000000000000000 ) ) ;
#13577 = VECTOR ( 'NONE', #19310, 1000.000000000000000 ) ;
#13578 = AXIS2_PLACEMENT_3D ( 'NONE', #7953, #17730, #11354 ) ;
#13579 = CARTESIAN_POINT ( 'NONE',  ( -27.29860958162435480, 65.74999999999997158, 5.347094680480812379 ) ) ;
#13580 = CONICAL_SURFACE ( 'NONE', #20674, 10.85470691220533190, 0.8171114040043576665 ) ;
#13581 = PLANE ( 'NONE',  #5361 ) ;
#13582 = PLANE ( 'NONE',  #13731 ) ;
#13583 = EDGE_CURVE ( 'NONE', #18388, #12727, #11997, .T. ) ;
#13584 = AXIS2_PLACEMENT_3D ( 'NONE', #7809, #20839, #2950 ) ;
#13585 = ORIENTED_EDGE ( 'NONE', *, *, #27, .T. ) ;
#13586 = CARTESIAN_POINT ( 'NONE',  ( 227.1472425980001333, 40.30537175372559489, -10.17395310825081012 ) ) ;
#13587 = DIRECTION ( 'NONE',  ( 0.8660254037844344888, 0.5000000000000069944, 0.000000000000000000 ) ) ;
#13588 = PLANE ( 'NONE',  #429 ) ;
#13589 = DIRECTION ( 'NONE',  ( 0.000000000000000000, 0.000000000000000000, 1.000000000000000000 ) ) ;
#13590 = FACE_OUTER_BOUND ( 'NONE', #4940, .T. ) ;
#13591 = FACE_OUTER_BOUND ( 'NONE', #18419, .T. ) ;
#13592 = EDGE_LOOP ( 'NONE', ( #14001, #10329, #7782, #3693 ) ) ;
#13593 = ADVANCED_FACE ( 'NONE', ( #647 ), #10263, .F. ) ;
#13594 = CARTESIAN_POINT ( 'NONE',  ( 81.85367731271401226, 60.34691469923900797, -0.3446091499246847212 ) ) ;
#13595 = CIRCLE ( 'NONE', #4448, 14.99999999999999645 ) ;
#13596 = ORIENTED_EDGE ( 'NONE', *, *, #2296, .T. ) ;
#13597 = CARTESIAN_POINT ( 'NONE',  ( 198.5498304622664989, 5.926496351342651181, -5.407152407593843968 ) ) ;
#13598 = VECTOR ( 'NONE', #20691, 1000.000000000000114 ) ;
#13599 = CARTESIAN_POINT ( 'NONE',  ( 80.06776404988029583, 51.44734343012801503, -6.071549608444867907 ) ) ;
#13600 = VECTOR ( 'NONE', #11307, 1000.000000000000114 ) ;
#13601 = ORIENTED_EDGE ( 'NONE', *, *, #13350, .F. ) ;
#13602 = CIRCLE ( 'NONE', #7483, 13.50000000000000178 ) ;
#13603 = SHAPE_DEFINITION_REPRESENTATION ( #15708, #9759 ) ;
#13604 = DIRECTION ( 'NONE',  ( 0.000000000000000000, 0.000000000000000000, 1.000000000000000000 ) ) ;
#13605 = ORIENTED_EDGE ( 'NONE', *, *, #17508, .F. ) ;
#13606 = CARTESIAN_POINT ( 'NONE',  ( 77.04324694534321338, 54.69866214318452080, -20.45431430911883908 ) ) ;
#13607 = DIRECTION ( 'NONE',  ( -0.5943026915289656431, -0.3431208189343725179, -0.7273736415730450711 ) ) ;
#13608 = DIRECTION ( 'NONE',  ( 0.8660254037844355990, 0.5000000000000051070, -1.748523119690306661E-16 ) ) ;
#13609 = LINE ( 'NONE', #463, #6073 ) ;
#13610 = ORIENTED_EDGE ( 'NONE', *, *, #17317, .F. ) ;
#13611 = CONICAL_SURFACE ( 'NONE', #8870, 13.07248899748297433, 0.6693469023067423196 ) ;
#13612 = CARTESIAN_POINT ( 'NONE',  ( 28.00000000000001066, 65.75000000000001421, 1.479896280015810639 ) ) ;
#13613 = CIRCLE ( 'NONE', #11235, 16.49999999999999645 ) ;
#13614 = CYLINDRICAL_SURFACE ( 'NONE', #2448, 12.47473710546057646 ) ;
#13615 = B_SPLINE_CURVE_WITH_KNOTS ( 'NONE', 3,
 ( #18773, #9001, #1177, #855 ),
 .UNSPECIFIED., .F., .F.,
 ( 4, 4 ),
 ( 3.603418170223495296E-07, 0.0008543460798012778587 ),
 .UNSPECIFIED. ) ;
#13616 = CARTESIAN_POINT ( 'NONE',  ( 218.0578026990161504, 37.02820936217296577, -16.57782486433068314 ) ) ;
#13617 = ORIENTED_EDGE ( 'NONE', *, *, #3937, .F. ) ;
#13618 = SURFACE_STYLE_USAGE ( .BOTH. , #15535 ) ;
#13619 = CARTESIAN_POINT ( 'NONE',  ( 37.85427444295662269, 178.3908428320656299, 11.00000000000001243 ) ) ;
#13620 = CARTESIAN_POINT ( 'NONE',  ( 203.3297164780629487, 6.518256075426767313E-05, -14.00000000000005507 ) ) ;
#13621 = CARTESIAN_POINT ( 'NONE',  ( 178.2433706042749009, 57.37193107572242923, -14.00000000000002842 ) ) ;
#13622 = COLOUR_RGB ( '',0.7921568627450980005, 0.8196078431372548767, 0.9333333333333333481 ) ;
#13624 = ORIENTED_EDGE ( 'NONE', *, *, #19087, .F. ) ;
#13623 = ORIENTED_EDGE ( 'NONE', *, *, #1986, .F. ) ;
#13625 = ORIENTED_EDGE ( 'NONE', *, *, #17867, .F. ) ;
#13626 = CARTESIAN_POINT ( 'NONE',  ( 0.000000000000000000, 2.342598717236900718, -4.057500000000001883 ) ) ;
#13627 = DIRECTION ( 'NONE',  ( -0.5000000000000047740, 0.8660254037844358210, 0.000000000000000000 ) ) ;
#13628 = CARTESIAN_POINT ( 'NONE',  ( -33.48683788045275378, 76.55850487625095013, -2.936742252775472739 ) ) ;
#13629 = AXIS2_PLACEMENT_3D ( 'NONE', #8612, #11698, #10291 ) ;
#13630 =( GEOMETRIC_REPRESENTATION_CONTEXT ( 3 ) GLOBAL_UNCERTAINTY_ASSIGNED_CONTEXT ( ( #1730 ) ) GLOBAL_UNIT_ASSIGNED_CONTEXT ( ( #2942, #9381, #1351 ) ) REPRESENTATION_CONTEXT ( 'NONE', 'WORKASPACE' ) );
#13631 = CARTESIAN_POINT ( 'NONE',  ( 26.99999999999999645, 65.00000000000000000, -12.50000000000000000 ) ) ;
#13632 = CARTESIAN_POINT ( 'NONE',  ( 198.2252501544971324, -1.168701404234412600, -16.84132998195068964 ) ) ;
#13633 = EDGE_LOOP ( 'NONE', ( #15132, #12196, #4638, #16580, #602 ) ) ;
#13634 = EDGE_CURVE ( 'NONE', #10224, #14892, #2166, .T. ) ;
#13635 = CARTESIAN_POINT ( 'NONE',  ( 82.20788507225606168, 63.93871732008117448, -25.46035155396378968 ) ) ;
#13636 = CARTESIAN_POINT ( 'NONE',  ( 59.05164960708168564, 85.13446652039156959, -14.98897224784199800 ) ) ;
#13637 = VERTEX_POINT ( 'NONE', #18243 ) ;
#13638 = CARTESIAN_POINT ( 'NONE',  ( 203.0529676813258106, 24.20295447737667516, -14.99132954693030229 ) ) ;
#13639 = CARTESIAN_POINT ( 'NONE',  ( 213.5401130648333492, 14.58114004716331280, -6.286464976499002155 ) ) ;
#13640 = VECTOR ( 'NONE', #11779, 1000.000000000000000 ) ;
#13641 = CARTESIAN_POINT ( 'NONE',  ( 219.1512096470114841, 35.13437297489623035, -18.24372585368654498 ) ) ;
#13642 = CYLINDRICAL_SURFACE ( 'NONE', #6742, 2.499999999999994671 ) ;
#13643 = CONICAL_SURFACE ( 'NONE', #3425, 1.499999999999990896, 0.8526294284052392536 ) ;
#13644 = DIRECTION ( 'NONE',  ( 1.000000000000000000, -0.000000000000000000, -0.000000000000000000 ) ) ;
#13646 = VERTEX_POINT ( 'NONE', #5189 ) ;
#13645 = ORIENTED_EDGE ( 'NONE', *, *, #19129, .T. ) ;
#13647 = ORIENTED_EDGE ( 'NONE', *, *, #15861, .T. ) ;
#13648 = CARTESIAN_POINT ( 'NONE',  ( 230.0624554316254091, 36.23554090207324663, -13.42327856638907058 ) ) ;
#13649 = CARTESIAN_POINT ( 'NONE',  ( 203.4540983502001836, 1.592568494036425530, -24.50020013040629863 ) ) ;
#13650 = ADVANCED_FACE ( 'NONE', ( #13590 ), #18137, .F. ) ;
#13651 = VERTEX_POINT ( 'NONE', #13372 ) ;
#13652 = CARTESIAN_POINT ( 'NONE',  ( 61.57468973143931379, 74.87077495648827608, -20.95977551465544764 ) ) ;
#13653 = CARTESIAN_POINT ( 'NONE',  ( 217.3629815419766942, 9.365266725128718051, -20.52105855319946670 ) ) ;
#13654 = ORIENTED_EDGE ( 'NONE', *, *, #6639, .F. ) ;
#13655 = DIRECTION ( 'NONE',  ( 0.8660254037844369313, 0.5000000000000029976, 3.053113317719180486E-16 ) ) ;
#13656 = LINE ( 'NONE', #5464, #4654 ) ;
#13657 = B_SPLINE_CURVE_WITH_KNOTS ( 'NONE', 3,
 ( #3020, #9465, #15969, #12780 ),
 .UNSPECIFIED., .F., .F.,
 ( 4, 4 ),
 ( 3.532015366477107683E-07, 0.0004524064433164963375 ),
 .UNSPECIFIED. ) ;
#13658 = CONICAL_SURFACE ( 'NONE', #5502, 13.07248899748297433, 0.6693469023067423196 ) ;
#13659 = ADVANCED_FACE ( 'NONE', ( #19820 ), #6994, .F. ) ;
#13660 = ADVANCED_FACE ( 'NONE', ( #3926 ), #20144, .T. ) ;
#13661 = DIRECTION ( 'NONE',  ( 0.000000000000000000, 0.9982500481053675490, -0.05913409725049680044 ) ) ;
#13662 = DIRECTION ( 'NONE',  ( -0.5000000000000051070, 0.8660254037844359321, -0.000000000000000000 ) ) ;
#13663 = CARTESIAN_POINT ( 'NONE',  ( -21.23313076374843078, 50.33498419130910406, -15.65462769131217513 ) ) ;
#13664 = CARTESIAN_POINT ( 'NONE',  ( -14.99999999999999645, 5.000000000000000000, -30.00000000000000000 ) ) ;
#13665 = ORIENTED_EDGE ( 'NONE', *, *, #9260, .T. ) ;
#13666 = DIRECTION ( 'NONE',  ( 1.000000000000000000, 0.000000000000000000, 0.000000000000000000 ) ) ;
#13667 = CARTESIAN_POINT ( 'NONE',  ( -27.29860958162435480, 64.25000000000000000, 5.347094680480811490 ) ) ;
#13668 = EDGE_CURVE ( 'NONE', #6975, #1937, #8805, .T. ) ;
#13670 = ORIENTED_EDGE ( 'NONE', *, *, #2278, .F. ) ;
#13669 = VERTEX_POINT ( 'NONE', #13482 ) ;
#13671 = AXIS2_PLACEMENT_3D ( 'NONE', #17203, #5945, #1304 ) ;
#13672 = CARTESIAN_POINT ( 'NONE',  ( 62.26115743202674224, 78.37397343634121682, -14.48362007552005437 ) ) ;
#13673 = ORIENTED_EDGE ( 'NONE', *, *, #1997, .F. ) ;
#13674 = ORIENTED_EDGE ( 'NONE', *, *, #17120, .T. ) ;
#13675 = EDGE_LOOP ( 'NONE', ( #1668, #7407, #16452, #2374, #6737, #13501, #12354, #7165, #6313 ) ) ;
#13676 = CARTESIAN_POINT ( 'NONE',  ( 89.99529059433416478, 168.0799536996104848, 26.00000000000001066 ) ) ;
#13677 = DIRECTION ( 'NONE',  ( -1.000000000000000000, -0.000000000000000000, -0.000000000000000000 ) ) ;
#13678 = ADVANCED_FACE ( 'NONE', ( #7212 ), #13271, .F. ) ;
#13679 = ORIENTED_EDGE ( 'NONE', *, *, #5617, .T. ) ;
#13680 = EDGE_LOOP ( 'NONE', ( #5061, #20685, #17380, #12293 ) ) ;
#13681 = DIRECTION ( 'NONE',  ( 0.5000000000000053291, -0.8660254037844355990, -2.220446049250312588E-16 ) ) ;
#13682 = ADVANCED_FACE ( 'NONE', ( #13694 ), #11675, .F. ) ;
#13683 = DIRECTION ( 'NONE',  ( -0.4999999999999995004, 0.8660254037844390407, 0.000000000000000000 ) ) ;
#13684 = CARTESIAN_POINT ( 'NONE',  ( 220.2180084519553134, 35.41797800104779270, -14.00000000000005507 ) ) ;
#13685 = VECTOR ( 'NONE', #9222, 1000.000000000000000 ) ;
#13686 = DIRECTION ( 'NONE',  ( -0.8528685319524408337, -0.4924038765061092282, -0.1736481776669271115 ) ) ;
#13687 = AXIS2_PLACEMENT_3D ( 'NONE', #8375, #15303, #15195 ) ;
#13688 =( BOUNDED_SURFACE ( )  B_SPLINE_SURFACE ( 3, 2, ( 
 ( #17611, #7637, #14133 ),
 ( #11035, #19096, #6040 ),
 ( #7530, #3084, #12637 ),
 ( #4768, #12528, #11250 ),
 ( #17719, #2880, #9317 ),
 ( #20463, #18991, #4568 ),
 ( #4470, #20669, #12434 ),
 ( #9426, #10931, #17400 ),
 ( #7740, #14239, #3184 ),
 ( #9636, #15922, #1393 ),
 ( #1081, #14021, #7841 ),
 ( #14343, #20775, #18888 ),
 ( #6243, #4666, #1598 ),
 ( #19593, #13254, #19699 ),
 ( #14658, #8143, #11660 ),
 ( #17923, #6872, #9938 ) ),
 .UNSPECIFIED., .F., .F., .F. ) 
 B_SPLINE_SURFACE_WITH_KNOTS ( ( 4, 2, 2, 2, 2, 2, 2, 4 ),
 ( 3, 3 ),
 ( 0.09394529277310079141, 0.09803747693844744315, 0.1000835690211207829, 0.1011066150624574389, 0.1021296611037941088, 0.1062218452691407744, 0.1082679373518141003, 0.1103140294344874262 ),
 ( 0.000000000000000000, 1.000000000000000000 ),
 .UNSPECIFIED. ) 
 GEOMETRIC_REPRESENTATION_ITEM ( )  RATIONAL_B_SPLINE_SURFACE ( (
 ( 1.000000000000000000, 0.7167790485004655876, 1.000000000000000000),
 ( 1.000000000000000000, 0.7312157917998172163, 1.000000000000000000),
 ( 1.000000000000000000, 0.7466500244729726843, 1.000000000000000000),
 ( 1.000000000000000000, 0.7689011243010781538, 1.000000000000000000),
 ( 1.000000000000000000, 0.7761748643737284015, 1.000000000000000000),
 ( 1.000000000000000000, 0.7866334538990542580, 1.000000000000000000),
 ( 1.000000000000000000, 0.7900487569768038787, 1.000000000000000000),
 ( 1.000000000000000000, 0.7966228133243151710, 1.000000000000000000),
 ( 1.000000000000000000, 0.7997907721098685974, 1.000000000000000000),
 ( 1.000000000000000000, 0.8149753752734353318, 1.000000000000000000),
 ( 1.000000000000000000, 0.8250225257834536974, 1.000000000000000000),
 ( 1.000000000000000000, 0.8359195949012505622, 1.000000000000000000),
 ( 1.000000000000000000, 0.8388534816486922230, 1.000000000000000000),
 ( 1.000000000000000000, 0.8430760250472538742, 1.000000000000000000),
 ( 1.000000000000000000, 0.8443918141124598931, 1.000000000000000000),
 ( 1.000000000000000000, 0.8449065510952337155, 1.000000000000000000) ) ) 
 REPRESENTATION_ITEM ( '' )  SURFACE ( )  );
#13689 = CARTESIAN_POINT ( 'NONE',  ( 26.00000000000000355, 5.616230220889761452E-16, -4.171999999999999709 ) ) ;
#13690 = DIRECTION ( 'NONE',  ( 0.5000000000000007772, -0.8660254037844381525, 0.000000000000000000 ) ) ;
#13691 = CARTESIAN_POINT ( 'NONE',  ( 62.36389338619030553, 105.9389375482328006, 4.000000000000000000 ) ) ;
#13692 = EDGE_CURVE ( 'NONE', #12370, #18332, #17745, .T. ) ;
#13693 = VERTEX_POINT ( 'NONE', #2770 ) ;
#13694 = FACE_OUTER_BOUND ( 'NONE', #20406, .T. ) ;
#13695 = DIRECTION ( 'NONE',  ( 0.4439426092011903302, -0.7689311547811511494, -0.4600650377311500949 ) ) ;
#13696 = ADVANCED_FACE ( 'NONE', ( #15605, #20457 ), #7308, .F. ) ;
#13697 = ORIENTED_EDGE ( 'NONE', *, *, #10450, .T. ) ;
#13698 = CARTESIAN_POINT ( 'NONE',  ( -2.446924783487210764, 65.74999999999998579, 3.020008312198914968 ) ) ;
#13699 = ORIENTED_EDGE ( 'NONE', *, *, #5004, .T. ) ;
#13700 = LINE ( 'NONE', #20151, #13872 ) ;
#13701 = DIRECTION ( 'NONE',  ( 6.608470384673549052E-16, -1.000000000000000000, 0.000000000000000000 ) ) ;
#13702 = EDGE_CURVE ( 'NONE', #15950, #1927, #10700, .T. ) ;
#13703 = DIRECTION ( 'NONE',  ( 1.000000000000000000, 0.000000000000000000, 0.000000000000000000 ) ) ;
#13704 = DIRECTION ( 'NONE',  ( -0.8660254037844360431, -0.5000000000000045519, -0.000000000000000000 ) ) ;
#13705 = ORIENTED_EDGE ( 'NONE', *, *, #9220, .F. ) ;
#13706 = CARTESIAN_POINT ( 'NONE',  ( 79.58925804534456461, 58.33401430123417697, -23.67724775046685437 ) ) ;
#13707 = ADVANCED_FACE ( 'NONE', ( #12424, #17082 ), #1074, .T. ) ;
#13708 = DIRECTION ( 'NONE',  ( -0.8660254037844357100, -0.5000000000000051070, 0.000000000000000000 ) ) ;
#13709 = FACE_OUTER_BOUND ( 'NONE', #20051, .T. ) ;
#13710 = CARTESIAN_POINT ( 'NONE',  ( 201.5617312735136579, 7.665418095488669259, -2.488895219275796933 ) ) ;
#13711 = VERTEX_POINT ( 'NONE', #17285 ) ;
#13712 = DIRECTION ( 'NONE',  ( 0.5000000000000051070, -0.8660254037844359321, 0.000000000000000000 ) ) ;
#13713 = AXIS2_PLACEMENT_3D ( 'NONE', #4701, #17648, #14794 ) ;
#13714 = EDGE_CURVE ( 'NONE', #5663, #19244, #14126, .T. ) ;
#13715 = CARTESIAN_POINT ( 'NONE',  ( 226.4210616241540208, 42.54261998698029146, -12.08027307405517448 ) ) ;
#13716 = DIRECTION ( 'NONE',  ( 0.8660254037844355990, 0.5000000000000054401, -1.599177586275613688E-14 ) ) ;
#13717 = ORIENTED_EDGE ( 'NONE', *, *, #14844, .F. ) ;
#13718 = LINE ( 'NONE', #2369, #691 ) ;
#13719 = CARTESIAN_POINT ( 'NONE',  ( 205.5965122587965084, 9.994899983462953941, -14.00000000000005507 ) ) ;
#13720 = DIRECTION ( 'NONE',  ( 0.000000000000000000, -1.000000000000000000, 0.000000000000000000 ) ) ;
#13721 = PLANE ( 'NONE',  #19236 ) ;
#13723 = ORIENTED_EDGE ( 'NONE', *, *, #14740, .T. ) ;
#13722 = ORIENTED_EDGE ( 'NONE', *, *, #14124, .T. ) ;
#13724 = ORIENTED_EDGE ( 'NONE', *, *, #3025, .F. ) ;
#13725 = CARTESIAN_POINT ( 'NONE',  ( 10.49211908931699178, 0.000000000000000000, 0.000000000000000000 ) ) ;
#13726 = SURFACE_SIDE_STYLE ('',( #15545 ) ) ;
#13727 = ORIENTED_EDGE ( 'NONE', *, *, #616, .F. ) ;
#13728 = CARTESIAN_POINT ( 'NONE',  ( 219.1254566829535975, 10.64043144601880897, -15.41218500610179198 ) ) ;
#13729 = ORIENTED_EDGE ( 'NONE', *, *, #6510, .T. ) ;
#13730 = DIRECTION ( 'NONE',  ( -0.8660254037844357100, -0.5000000000000049960, 0.000000000000000000 ) ) ;
#13731 = AXIS2_PLACEMENT_3D ( 'NONE', #17930, #14871, #11670 ) ;
#13732 = CARTESIAN_POINT ( 'NONE',  ( -28.35621592425299653, 6.482730417836661374, 1.947608771879208556 ) ) ;
#13733 = DIRECTION ( 'NONE',  ( 0.4084849465052216022, -0.7075166814740940779, 0.5766803221148710801 ) ) ;
#13734 = ORIENTED_EDGE ( 'NONE', *, *, #814, .T. ) ;
#13735 = CARTESIAN_POINT ( 'NONE',  ( 79.67828149300846974, 55.39867050251828573, -21.30364596931944376 ) ) ;
#13736 = DIRECTION ( 'NONE',  ( 0.8660254037844355990, 0.5000000000000054401, 0.000000000000000000 ) ) ;
#13737 = EDGE_LOOP ( 'NONE', ( #12665, #18330, #19518, #17537, #15219 ) ) ;
#13738 = CARTESIAN_POINT ( 'NONE',  ( 202.2784612918522100, 25.28746711354437693, -15.49033546657680915 ) ) ;
#13739 = CARTESIAN_POINT ( 'NONE',  ( 205.9193846489986015, 10.18131044486001535, -16.32385667531026741 ) ) ;
#13740 = CARTESIAN_POINT ( 'NONE',  ( -34.00000000000000711, 64.25000000000000000, 2.481238266578627449 ) ) ;
#13741 = CARTESIAN_POINT ( 'NONE',  ( 196.9187795697884269, 4.984808679508447860, -7.425127016398286983 ) ) ;
#13742 = DIRECTION ( 'NONE',  ( 0.5000000000000055511, -0.8660254037844353769, 2.775557561562890735E-17 ) ) ;
#13743 = VECTOR ( 'NONE', #16033, 1000.000000000000000 ) ;
#13744 = VERTEX_POINT ( 'NONE', #4144 ) ;
#13745 = ORIENTED_EDGE ( 'NONE', *, *, #11961, .F. ) ;
#13746 = AXIS2_PLACEMENT_3D ( 'NONE', #905, #3866, #13736 ) ;
#13747 = EDGE_LOOP ( 'NONE', ( #7681, #2563, #11745, #13195, #14488 ) ) ;
#13748 = CARTESIAN_POINT ( 'NONE',  ( 221.6316662300224607, 32.32157772951582331, -15.10067325715091968 ) ) ;
#13749 = FACE_OUTER_BOUND ( 'NONE', #12703, .T. ) ;
#13750 = VERTEX_POINT ( 'NONE', #2665 ) ;
#13751 = ORIENTED_EDGE ( 'NONE', *, *, #4342, .T. ) ;
#13752 = ADVANCED_FACE ( 'NONE', ( #20246 ), #18669, .F. ) ;
#13753 = DIRECTION ( 'NONE',  ( 0.8660254037844372643, 0.5000000000000027756, -0.000000000000000000 ) ) ;
#13754 = CARTESIAN_POINT ( 'NONE',  ( 172.0049095375684090, -3.964873019432338275, -29.00000000000001066 ) ) ;
#13755 = PLANE ( 'NONE',  #7989 ) ;
#13756 = DIRECTION ( 'NONE',  ( -0.5000000000000045519, 0.8660254037844360431, 0.000000000000000000 ) ) ;
#13757 = CARTESIAN_POINT ( 'NONE',  ( 199.4075733045063146, 6.421714412205289157, -4.379064819896086647 ) ) ;
#13758 = VERTEX_POINT ( 'NONE', #9104 ) ;
#13759 = CIRCLE ( 'NONE', #16453, 15.00000000000000000 ) ;
#13760 = CIRCLE ( 'NONE', #14457, 13.99999999999999822 ) ;
#13761 = PLANE ( 'NONE',  #325 ) ;
#13762 = EDGE_CURVE ( 'NONE', #9756, #6104, #1830, .T. ) ;
#13763 = CARTESIAN_POINT ( 'NONE',  ( 209.4067366129695529, 3.387278741123676440, -14.00000000000005507 ) ) ;
#13764 = CARTESIAN_POINT ( 'NONE',  ( -15.26367225750305856, 49.50789260602288522, -12.48397009176186145 ) ) ;
#13765 = CARTESIAN_POINT ( 'NONE',  ( -31.74999999999995737, 0.000000000000000000, 0.000000000000000000 ) ) ;
#13766 = ORIENTED_EDGE ( 'NONE', *, *, #16868, .F. ) ;
#13767 = DIRECTION ( 'NONE',  ( 0.000000000000000000, 0.000000000000000000, -1.000000000000000000 ) ) ;
#13768 = LINE ( 'NONE', #18747, #20180 ) ;
#13770 = VERTEX_POINT ( 'NONE', #18880 ) ;
#13769 = ORIENTED_EDGE ( 'NONE', *, *, #14862, .F. ) ;
#13771 = AXIS2_PLACEMENT_3D ( 'NONE', #4598, #19327, #17536 ) ;
#13772 = EDGE_LOOP ( 'NONE', ( #18422, #16263, #11392, #9316 ) ) ;
#13773 = CARTESIAN_POINT ( 'NONE',  ( 198.5809828321035013, -0.9633190470588108845, -9.788772202513250420 ) ) ;
#13774 = CARTESIAN_POINT ( 'NONE',  ( 60.49916866905066115, 75.33328221149844239, -20.42012703083461389 ) ) ;
#13775 = B_SPLINE_CURVE_WITH_KNOTS ( 'NONE', 3,
 ( #9499, #1566, #14410, #18953 ),
 .UNSPECIFIED., .F., .F.,
 ( 4, 4 ),
 ( 2.448070629158399379E-07, 0.0005857331628025336722 ),
 .UNSPECIFIED. ) ;
#13776 = EDGE_CURVE ( 'NONE', #8267, #19987, #10599, .T. ) ;
#13777 = ORIENTED_EDGE ( 'NONE', *, *, #7902, .T. ) ;
#13778 = VECTOR ( 'NONE', #11611, 1000.000000000000227 ) ;
#13779 = EDGE_CURVE ( 'NONE', #2710, #16780, #2852, .T. ) ;
#13780 = ORIENTED_EDGE ( 'NONE', *, *, #10639, .T. ) ;
#13781 = CARTESIAN_POINT ( 'NONE',  ( 198.8157711536554189, -0.5701500946419610916, -8.415281845791808379 ) ) ;
#13782 = CARTESIAN_POINT ( 'NONE',  ( 211.4194833127196489, 27.45139579749023540, -14.00000000000004974 ) ) ;
#13783 = ORIENTED_EDGE ( 'NONE', *, *, #3916, .T. ) ;
#13784 = ORIENTED_EDGE ( 'NONE', *, *, #3642, .T. ) ;
#13785 = CARTESIAN_POINT ( 'NONE',  ( 193.6336827526812101, 7.212155065240265728, -15.39542905462715083 ) ) ;
#13786 = CARTESIAN_POINT ( 'NONE',  ( 213.9922241104001444, 18.96616439842760471, -12.64773574313060678 ) ) ;
#13787 = CARTESIAN_POINT ( 'NONE',  ( -31.74999999999995737, 0.000000000000000000, 0.000000000000000000 ) ) ;
#13788 = CARTESIAN_POINT ( 'NONE',  ( -12.02764249544091868, 18.15304305180008271, 11.85355413814486703 ) ) ;
#13789 = VECTOR ( 'NONE', #9198, 999.9999999999998863 ) ;
#13790 = CARTESIAN_POINT ( 'NONE',  ( 214.7465214175448125, 15.27766023435388298, -8.669480444820855780 ) ) ;
#13791 = DIRECTION ( 'NONE',  ( -0.7743856023693594937, 0.000000000000000000, 0.6327139470906613106 ) ) ;
#13792 = AXIS2_PLACEMENT_3D ( 'NONE', #20767, #10921, #17393 ) ;
#13793 = CARTESIAN_POINT ( 'NONE',  ( 227.9553588074475670, 39.88513931160575510, -14.00000000000005507 ) ) ;
#13794 = EDGE_CURVE ( 'NONE', #1224, #17966, #15507, .T. ) ;
#13795 = ORIENTED_EDGE ( 'NONE', *, *, #20040, .T. ) ;
#13796 = CARTESIAN_POINT ( 'NONE',  ( -33.48481952675159334, 76.25000000000001421, -2.578432583507806353 ) ) ;
#13797 = DIRECTION ( 'NONE',  ( -0.9679941405060890069, 0.000000000000000000, 0.2509727952306343712 ) ) ;
#13798 = CARTESIAN_POINT ( 'NONE',  ( 30.92607121268107306, 174.3908428320655446, 11.00000000000001243 ) ) ;
#13799 = ORIENTED_EDGE ( 'NONE', *, *, #10164, .F. ) ;
#13800 = CYLINDRICAL_SURFACE ( 'NONE', #10853, 16.49999999999999645 ) ;
#13801 = EDGE_CURVE ( 'NONE', #10792, #11033, #12520, .T. ) ;
#13802 = ORIENTED_EDGE ( 'NONE', *, *, #20802, .T. ) ;
#13803 = DIRECTION ( 'NONE',  ( 0.5000000000000044409, -0.8660254037844360431, -0.000000000000000000 ) ) ;
#13804 = CARTESIAN_POINT ( 'NONE',  ( 77.55491039835763445, 55.40237803623692514, -3.717510863212275307 ) ) ;
#13805 = EDGE_CURVE ( 'NONE', #18096, #9213, #7736, .T. ) ;
#13806 = VECTOR ( 'NONE', #6225, 1000.000000000000000 ) ;
#13807 = EDGE_CURVE ( 'NONE', #7763, #10335, #2454, .T. ) ;
#13808 = AXIS2_PLACEMENT_3D ( 'NONE', #10478, #2556, #9207 ) ;
#13809 = CARTESIAN_POINT ( 'NONE',  ( 228.3393538449945481, 39.22004039672007281, -10.17395310825082611 ) ) ;
#13810 = EDGE_CURVE ( 'NONE', #15276, #14622, #6703, .T. ) ;
#13811 = ORIENTED_EDGE ( 'NONE', *, *, #20234, .F. ) ;
#13812 = SURFACE_STYLE_FILL_AREA ( #15730 ) ;
#13813 = CARTESIAN_POINT ( 'NONE',  ( 226.7270994320308546, 41.68607787873453674, -10.98877789909423619 ) ) ;
#13814 = PLANE ( 'NONE',  #20490 ) ;
#13815 = LINE ( 'NONE', #12442, #12896 ) ;
#13816 = FACE_OUTER_BOUND ( 'NONE', #5214, .T. ) ;
#13817 = ADVANCED_FACE ( 'NONE', ( #2872 ), #20661, .F. ) ;
#13818 = DIRECTION ( 'NONE',  ( 0.000000000000000000, 0.000000000000000000, -1.000000000000000000 ) ) ;
#13819=STYLED_ITEM('',(#20967),#17599);
#13820 = CARTESIAN_POINT ( 'NONE',  ( 199.5603494194345444, -0.9130877231049959741, -19.34736286182874565 ) ) ;
#13821 = PRODUCT ( 'socket head cap screw_iso_ISO 4762 M8 x 35 - 35N', 'socket head cap screw_iso_ISO 4762 M8 x 35 - 35N', '', ( #17403 ) ) ;
#13822 = ORIENTED_EDGE ( 'NONE', *, *, #9402, .T. ) ;
#13823 = FILL_AREA_STYLE_COLOUR ( '', #4745 ) ;
#13824 = EDGE_CURVE ( 'NONE', #10811, #2349, #18418, .T. ) ;
#13826 = CARTESIAN_POINT ( 'NONE',  ( 5.000000000000004441, 7.027796151710827388, -4.057500000000009877 ) ) ;
#13825 = CIRCLE ( 'NONE', #2989, 8.000000000000058620 ) ;
#13827 = DIRECTION ( 'NONE',  ( 0.8660254037844372643, 0.5000000000000027756, -0.000000000000000000 ) ) ;
#13828 = EDGE_CURVE ( 'NONE', #9199, #14589, #16327, .T. ) ;
#13829 = LINE ( 'NONE', #2372, #12838 ) ;
#13831 = ORIENTED_EDGE ( 'NONE', *, *, #16379, .T. ) ;
#13830 = ORIENTED_EDGE ( 'NONE', *, *, #4556, .T. ) ;
#13832 = ORIENTED_EDGE ( 'NONE', *, *, #490, .T. ) ;
#13833 = CARTESIAN_POINT ( 'NONE',  ( -12.23735126049118627, 11.79085703297993248, 11.92262888347531913 ) ) ;
#13834 = ORIENTED_EDGE ( 'NONE', *, *, #11700, .F. ) ;
#13835 = CARTESIAN_POINT ( 'NONE',  ( -19.71973103665720117, 79.99808926845247470, -12.23885522625830014 ) ) ;
#13836 = UNCERTAINTY_MEASURE_WITH_UNIT (LENGTH_MEASURE( 1.000000000000000082E-05 ), #488, 'distance_accuracy_value', 'NONE');
#13837 = EDGE_CURVE ( 'NONE', #18324, #7529, #4562, .T. ) ;
#13838 = CARTESIAN_POINT ( 'NONE',  ( 105.1989074543211871, 189.2062061502930135, 11.00000000000001066 ) ) ;
#13839 = VECTOR ( 'NONE', #10612, 1000.000000000000114 ) ;
#13840 = CARTESIAN_POINT ( 'NONE',  ( 208.4761278624580711, 5.007259451653140125, -14.00000000000005507 ) ) ;
#13841 = VERTEX_POINT ( 'NONE', #6439 ) ;
#13842 = CARTESIAN_POINT ( 'NONE',  ( 229.5134838794282643, 37.18638752238859269, -15.84136033874758454 ) ) ;
#13843 = CARTESIAN_POINT ( 'NONE',  ( 194.7177224586705222, 20.69538101841223821, -14.00000000000005329 ) ) ;
#13844 = EDGE_CURVE ( 'NONE', #1588, #11978, #9524, .T. ) ;
#13845 = ORIENTED_EDGE ( 'NONE', *, *, #11484, .F. ) ;
#13846 = DIRECTION ( 'NONE',  ( -0.8660254037844361541, -0.5000000000000045519, -4.336808689942050770E-16 ) ) ;
#13847 = DIRECTION ( 'NONE',  ( 0.5000000000000044409, -0.8660254037844360431, -4.006172263299080068E-16 ) ) ;
#13848 = DIRECTION ( 'NONE',  ( -0.4330127018922213522, -0.2500000000000047740, -0.8660254037844362651 ) ) ;
#13849 = LINE ( 'NONE', #15354, #7102 ) ;
#13850 = CARTESIAN_POINT ( 'NONE',  ( 206.7320635740233854, 14.77450875839051925, -25.34310559273333396 ) ) ;
#13851 = AXIS2_PLACEMENT_3D ( 'NONE', #5724, #12221, #18687 ) ;
#13853 = ORIENTED_EDGE ( 'NONE', *, *, #6378, .F. ) ;
#13852 = ORIENTED_EDGE ( 'NONE', *, *, #18818, .T. ) ;
#13854 = ORIENTED_EDGE ( 'NONE', *, *, #17585, .F. ) ;
#13855 = CARTESIAN_POINT ( 'NONE',  ( 89.99529059433416478, 168.0799536996104848, 26.00000000000001066 ) ) ;
#13856 = ADVANCED_FACE ( 'NONE', ( #14652 ), #16025, .T. ) ;
#13857 = DIRECTION ( 'NONE',  ( 0.03412120668233437071, -0.05909966358936864089, -0.9976687691905390398 ) ) ;
#13858 = PRODUCT_DEFINITION_FORMATION_WITH_SPECIFIED_SOURCE ( 'ANY', '', #16509, .NOT_KNOWN. ) ;
#13859 = EDGE_LOOP ( 'NONE', ( #5167, #2117, #71, #2097 ) ) ;
#13860 = EDGE_LOOP ( 'NONE', ( #19427, #19139 ) ) ;
#13861 = VERTEX_POINT ( 'NONE', #20863 ) ;
#13862 = CARTESIAN_POINT ( 'NONE',  ( -16.66506943655450357, 10.13295816235035751, 12.48647880216494421 ) ) ;
#13863 = FACE_OUTER_BOUND ( 'NONE', #20545, .T. ) ;
#13864 = FACE_OUTER_BOUND ( 'NONE', #14291, .T. ) ;
#13865 = CARTESIAN_POINT ( 'NONE',  ( 84.01452848080126046, 118.4389375482328859, 55.99999999999997868 ) ) ;
#13866 = CARTESIAN_POINT ( 'NONE',  ( -20.29791675083326652, 66.10905085997984543, -2.555169535221540222 ) ) ;
#13867 = ORIENTED_EDGE ( 'NONE', *, *, #13958, .T. ) ;
#13868 = DIRECTION ( 'NONE',  ( 0.03412120668233696585, -0.05909966358936712821, -0.9976687691905389288 ) ) ;
#13869 = DIRECTION ( 'NONE',  ( 0.6123724356957944703, 0.3535533905932780607, 0.7071067811865454633 ) ) ;
#13870 = CARTESIAN_POINT ( 'NONE',  ( -24.22102634534772392, 45.00409005278715568, -9.441307004238941758 ) ) ;
#13871 = CARTESIAN_POINT ( 'NONE',  ( 209.2023654653594349, 5.168939075417601003, -1.722272971484202220 ) ) ;
#13872 = VECTOR ( 'NONE', #15201, 1000.000000000000000 ) ;
#13873 = LINE ( 'NONE', #8776, #1843 ) ;
#13874 = CARTESIAN_POINT ( 'NONE',  ( -28.49821372255547658, 48.76782331758764855, -0.5569301972970369663 ) ) ;
#13876 = EDGE_LOOP ( 'NONE', ( #13382, #10935, #4097, #2599 ) ) ;
#13875 = VERTEX_POINT ( 'NONE', #6337 ) ;
#13877 = CARTESIAN_POINT ( 'NONE',  ( 208.0154570403102241, 11.39147840422473479, -11.03569519926165654 ) ) ;
#13878 = DIRECTION ( 'NONE',  ( 0.2282907716811782561, 0.9735929968755999697, 0.000000000000000000 ) ) ;
#13879 = ORIENTED_EDGE ( 'NONE', *, *, #16554, .T. ) ;
#13880 = VERTEX_POINT ( 'NONE', #14334 ) ;
#13881 = FACE_OUTER_BOUND ( 'NONE', #19186, .T. ) ;
#13882 = CARTESIAN_POINT ( 'NONE',  ( -29.73649742176619881, 50.04042210092456600, -11.28552931171784302 ) ) ;
#13883 = VECTOR ( 'NONE', #14285, 1000.000000000000227 ) ;
#13884 = CARTESIAN_POINT ( 'NONE',  ( 190.1694833127194499, 64.25747545832879837, -14.00000000000006395 ) ) ;
#13885 = VECTOR ( 'NONE', #5660, 1000.000000000000114 ) ;
#13886 = VERTEX_POINT ( 'NONE', #12941 ) ;
#13887 = ORIENTED_EDGE ( 'NONE', *, *, #10092, .T. ) ;
#13888 = EDGE_CURVE ( 'NONE', #17291, #20129, #14433, .T. ) ;
#13889 = CARTESIAN_POINT ( 'NONE',  ( 219.3321254432009368, 36.95237238177238481, -10.52303454827236884 ) ) ;
#13890 = LINE ( 'NONE', #17172, #15853 ) ;
#13891 = CARTESIAN_POINT ( 'NONE',  ( 214.0593366061550569, 19.00491181591769418, -13.97827067520052324 ) ) ;
#13892 = DIRECTION ( 'NONE',  ( -0.8660254037844361541, -0.5000000000000044409, 5.976026924694052093E-17 ) ) ;
#13893 = EDGE_CURVE ( 'NONE', #3402, #8955, #819, .T. ) ;
#13894 = CARTESIAN_POINT ( 'NONE',  ( -15.99999999999999289, 64.25000000000000000, 12.50000000000000000 ) ) ;
#13895 = CARTESIAN_POINT ( 'NONE',  ( -28.48915680482256008, 80.00000000000000000, 0.5205403966592370146 ) ) ;
#13896 = FACE_OUTER_BOUND ( 'NONE', #8783, .T. ) ;
#13897 = CARTESIAN_POINT ( 'NONE',  ( -28.48915680482256363, 80.00000000000001421, 0.5205403966592334619 ) ) ;
#13898 = AXIS2_PLACEMENT_3D ( 'NONE', #11182, #17662, #6389 ) ;
#13899 = DIRECTION ( 'NONE',  ( -1.000000000000000000, -0.000000000000000000, -0.000000000000000000 ) ) ;
#13900 = DIRECTION ( 'NONE',  ( 0.5000000000000044409, -0.8660254037844360431, -0.000000000000000000 ) ) ;
#13901 = ORIENTED_EDGE ( 'NONE', *, *, #4373, .F. ) ;
#13902 = CARTESIAN_POINT ( 'NONE',  ( -2.653101600560879625, 65.75000000000000000, 3.131020379152388067 ) ) ;
#13903 = AXIS2_PLACEMENT_3D ( 'NONE', #20253, #18361, #10605 ) ;
#13904 = ORIENTED_EDGE ( 'NONE', *, *, #6043, .F. ) ;
#13905 = ORIENTED_EDGE ( 'NONE', *, *, #7174, .F. ) ;
#13906 = FACE_OUTER_BOUND ( 'NONE', #9314, .T. ) ;
#13907 = DIRECTION ( 'NONE',  ( -0.8660254037844361541, -0.5000000000000045519, 5.976026924694053325E-17 ) ) ;
#13908 = AXIS2_PLACEMENT_3D ( 'NONE', #13140, #19584, #5062 ) ;
#13909 = VECTOR ( 'NONE', #14876, 1000.000000000000114 ) ;
#13910 = EDGE_CURVE ( 'NONE', #16503, #1328, #12750, .T. ) ;
#13911 = DIRECTION ( 'NONE',  ( 1.000000000000000000, 0.000000000000000000, 0.000000000000000000 ) ) ;
#13912 = AXIS2_PLACEMENT_3D ( 'NONE', #6316, #4944, #9911 ) ;
#13913 = CIRCLE ( 'NONE', #5099, 4.999999999999995559 ) ;
#13914 = DIRECTION ( 'NONE',  ( -0.8404609622712050365, 0.000000000000000000, -0.5418720982834971389 ) ) ;
#13915 = ORIENTED_EDGE ( 'NONE', *, *, #12483, .T. ) ;
#13916 = DIRECTION ( 'NONE',  ( 0.5000000000000046629, -0.8660254037844360431, -4.006172263299081054E-16 ) ) ;
#13917 = DIRECTION ( 'NONE',  ( -0.8660254037844378194, -0.5000000000000013323, -0.000000000000000000 ) ) ;
#13918 = DIRECTION ( 'NONE',  ( -1.000000000000000000, 0.000000000000000000, 0.000000000000000000 ) ) ;
#13919 = FACE_OUTER_BOUND ( 'NONE', #13592, .T. ) ;
#13920 = AXIS2_PLACEMENT_3D ( 'NONE', #2013, #6549, #8461 ) ;
#13921 = ADVANCED_FACE ( 'NONE', ( #8245 ), #14751, .T. ) ;
#13922 = B_SPLINE_CURVE_WITH_KNOTS ( 'NONE', 3,
 ( #12984, #16367, #6279, #3217 ),
 .UNSPECIFIED., .F., .F.,
 ( 4, 4 ),
 ( 7.831744291011048613E-05, 0.0007509682349631222791 ),
 .UNSPECIFIED. ) ;
#13923 = EDGE_CURVE ( 'NONE', #423, #18235, #111, .T. ) ;
#13924 = DIRECTION ( 'NONE',  ( 0.000000000000000000, -0.9841898184435641239, -0.1771169141330785901 ) ) ;
#13925 = VECTOR ( 'NONE', #11114, 1000.000000000000000 ) ;
#13926 = CARTESIAN_POINT ( 'NONE',  ( 216.3355731942785951, 15.66405044361498788, -16.89203719259520753 ) ) ;
#13927 = CARTESIAN_POINT ( 'NONE',  ( 226.2377201494591077, 42.53370766032038119, -12.03677242795825109 ) ) ;
#13928 = CARTESIAN_POINT ( 'NONE',  ( 205.5374615299400602, 3.053005801749057113, -2.216907231065453399 ) ) ;
#13929 = ORIENTED_EDGE ( 'NONE', *, *, #17019, .F. ) ;
#13930 = CIRCLE ( 'NONE', #4774, 12.47473710546057823 ) ;
#13931 = AXIS2_PLACEMENT_3D ( 'NONE', #16502, #20201, #11840 ) ;
#13932 = CARTESIAN_POINT ( 'NONE',  ( 42.39721438298049350, 244.5222400402098231, -8.999999999999973355 ) ) ;
#13933 = LINE ( 'NONE', #20697, #9830 ) ;
#13934 = AXIS2_PLACEMENT_3D ( 'NONE', #11809, #13720, #16578 ) ;
#13935 = EDGE_CURVE ( 'NONE', #17399, #12993, #16216, .T. ) ;
#13936 = CARTESIAN_POINT ( 'NONE',  ( 228.1017308963826622, 39.63161541676052479, -10.43865930680574827 ) ) ;
#13937 = DIRECTION ( 'NONE',  ( -0.8660254037844358210, -0.5000000000000049960, 0.000000000000000000 ) ) ;
#13939 = VERTEX_POINT ( 'NONE', #205 ) ;
#13938 = VERTEX_POINT ( 'NONE', #1691 ) ;
#13940 = ORIENTED_EDGE ( 'NONE', *, *, #5872, .T. ) ;
#13941 = CARTESIAN_POINT ( 'NONE',  ( 227.9553588074475954, 39.88513931160571957, -14.00000000000005507 ) ) ;
#13942 = PRESENTATION_STYLE_ASSIGNMENT (( #6066 ) ) ;
#13943 = VERTEX_POINT ( 'NONE', #13043 ) ;
#13944 = CARTESIAN_POINT ( 'NONE',  ( -22.46405759164546367, 79.97811033489706745, -11.66317476315385626 ) ) ;
#13945 = EDGE_CURVE ( 'NONE', #3166, #9370, #19089, .T. ) ;
#13946 = AXIS2_PLACEMENT_3D ( 'NONE', #7137, #15125, #18495 ) ;
#13947 = CARTESIAN_POINT ( 'NONE',  ( 199.6382066537783260, 23.53622389300110385, -14.00000000000005507 ) ) ;
#13948 = B_SPLINE_CURVE_WITH_KNOTS ( 'NONE', 3,
 ( #16599, #8644, #3872, #2086, #911, #7154, #500, #19984, #15041, #5445, #13430, #808, #15247, #7258, #11945, #18404 ),
 .UNSPECIFIED., .F., .F.,
 ( 4, 2, 2, 2, 2, 2, 2, 4 ),
 ( 1.398578778534940505E-17, 0.0004899730491125216594, 0.0009799460982250292242, 0.001469919147337537006, 0.001959892196450044571, 0.002939838294675023271, 0.003429811343787525849, 0.003919784392900028426 ),
 .UNSPECIFIED. ) ;
#13949 = CIRCLE ( 'NONE', #1083, 1.499999999999999556 ) ;
#13950 = CARTESIAN_POINT ( 'NONE',  ( 195.7860920451057325, 4.153841328041666614, -9.848357292554023701 ) ) ;
#13951 = EDGE_CURVE ( 'NONE', #5368, #14969, #896, .T. ) ;
#13952 = AXIS2_PLACEMENT_3D ( 'NONE', #889, #8832, #3637 ) ;
#13953 = CARTESIAN_POINT ( 'NONE',  ( 218.4231237361075841, 38.52680952262490166, -12.46964089162983313 ) ) ;
#13954 = ORIENTED_EDGE ( 'NONE', *, *, #5736, .F. ) ;
#13955 = LINE ( 'NONE', #1613, #15943 ) ;
#13956 = CARTESIAN_POINT ( 'NONE',  ( 217.8444015856884164, 37.39783093284837179, -10.88971489487115996 ) ) ;
#13957 = EDGE_CURVE ( 'NONE', #11977, #13235, #1432, .T. ) ;
#13958 = EDGE_CURVE ( 'NONE', #6373, #7969, #12414, .T. ) ;
#13959 = DIRECTION ( 'NONE',  ( 0.000000000000000000, 0.000000000000000000, 1.000000000000000000 ) ) ;
#13960 = CARTESIAN_POINT ( 'NONE',  ( 215.6932043811731603, 15.82422789824195242, -11.22353489230414958 ) ) ;
#13961 = VECTOR ( 'NONE', #8066, 1000.000000000000000 ) ;
#13962 = DIRECTION ( 'NONE',  ( -1.000000000000000000, -0.000000000000000000, -0.000000000000000000 ) ) ;
#13963 = EDGE_CURVE ( 'NONE', #10440, #8359, #16459, .T. ) ;
#13965 = ORIENTED_EDGE ( 'NONE', *, *, #18328, .F. ) ;
#13964 = ORIENTED_EDGE ( 'NONE', *, *, #4483, .F. ) ;
#13966 = ORIENTED_EDGE ( 'NONE', *, *, #8206, .T. ) ;
#13967 = CARTESIAN_POINT ( 'NONE',  ( 221.4218408946551619, 31.20152428872390615, -13.99751724578391432 ) ) ;
#13968 = B_SPLINE_CURVE_WITH_KNOTS ( 'NONE', 3,
 ( #5619, #17300, #18574, #10817 ),
 .UNSPECIFIED., .F., .F.,
 ( 4, 4 ),
 ( 1.468788439227401785E-06, 0.0005869571441788386116 ),
 .UNSPECIFIED. ) ;
#13969 = AXIS2_PLACEMENT_3D ( 'NONE', #1661, #7901, #12905 ) ;
#13970 = ORIENTED_EDGE ( 'NONE', *, *, #5201, .T. ) ;
#13971 = ORIENTED_EDGE ( 'NONE', *, *, #15986, .T. ) ;
#13972 = VERTEX_POINT ( 'NONE', #15912 ) ;
#13973 = CARTESIAN_POINT ( 'NONE',  ( 709.3577481411962253, -862.5451554485315455, -14.00000000000005507 ) ) ;
#13974 = FACE_OUTER_BOUND ( 'NONE', #19325, .T. ) ;
#13975 = CARTESIAN_POINT ( 'NONE',  ( 77.00490953756764156, 160.5799536996104280, 21.00000000000000711 ) ) ;
#13976 = EDGE_CURVE ( 'NONE', #4359, #10891, #10344, .T. ) ;
#13977 = CARTESIAN_POINT ( 'NONE',  ( -20.99999999999998224, 15.09941697557068530, 11.45643923738960446 ) ) ;
#13978 = DIRECTION ( 'NONE',  ( 0.000000000000000000, 0.000000000000000000, 1.000000000000000000 ) ) ;
#13979 = ORIENTED_EDGE ( 'NONE', *, *, #1148, .T. ) ;
#13980 = CARTESIAN_POINT ( 'NONE',  ( 229.6508453308915705, 36.62200143348649561, -14.54471643454063745 ) ) ;
#13981 = EDGE_CURVE ( 'NONE', #13875, #10891, #13410, .T. ) ;
#13982 = CIRCLE ( 'NONE', #18036, 17.50000000000000000 ) ;
#13983 = CIRCLE ( 'NONE', #8543, 11.98469917212512215 ) ;
#13984 = CARTESIAN_POINT ( 'NONE',  ( -20.71357962313245693, 45.34957306837157631, -11.59763734586043427 ) ) ;
#13985 = CARTESIAN_POINT ( 'NONE',  ( 31.00000000000000711, 65.00000000000000000, -2.500000000000005773 ) ) ;
#13986 = CARTESIAN_POINT ( 'NONE',  ( 215.2753377405919650, 15.22894589946059440, -19.53076827296978024 ) ) ;
#13987 = CARTESIAN_POINT ( 'NONE',  ( -27.58972166001723636, 58.88968531714240129, 4.685586124710503952 ) ) ;
#13989 = EDGE_LOOP ( 'NONE', ( #5097, #7776, #6929, #6730 ) ) ;
#13988 = ORIENTED_EDGE ( 'NONE', *, *, #20871, .F. ) ;
#13990 = DIRECTION ( 'NONE',  ( 0.000000000000000000, 0.000000000000000000, -1.000000000000000000 ) ) ;
#13991 = CARTESIAN_POINT ( 'NONE',  ( 205.2286857969292839, 9.782535276688834713, -12.71431551095683332 ) ) ;
#13992 = DIRECTION ( 'NONE',  ( -0.2597919750177185572, 0.4499729001293500397, 0.8544194045464879039 ) ) ;
#13993 = ORIENTED_EDGE ( 'NONE', *, *, #17828, .T. ) ;
#13994 = ORIENTED_EDGE ( 'NONE', *, *, #17179, .F. ) ;
#13995 = CARTESIAN_POINT ( 'NONE',  ( 28.00000000000001066, 65.75000000000001421, -1.525597966175989972 ) ) ;
#13996 = DIRECTION ( 'NONE',  ( 0.8660254037844357100, 0.5000000000000052180, 0.000000000000000000 ) ) ;
#13997 = CARTESIAN_POINT ( 'NONE',  ( -32.49130957492637606, 50.81462085746833424, -7.575237087458418728 ) ) ;
#13998 = DIRECTION ( 'NONE',  ( -0.5000000000000047740, 0.8660254037844358210, 0.000000000000000000 ) ) ;
#13999 = CIRCLE ( 'NONE', #18386, 3.461721407990061117 ) ;
#14000 = ORIENTED_EDGE ( 'NONE', *, *, #1720, .T. ) ;
#14001 = ORIENTED_EDGE ( 'NONE', *, *, #13306, .T. ) ;
#14002 = FACE_OUTER_BOUND ( 'NONE', #10625, .T. ) ;
#14003 = ORIENTED_EDGE ( 'NONE', *, *, #18227, .F. ) ;
#14004 = CARTESIAN_POINT ( 'NONE',  ( 218.6027909648456387, 37.56774357859059421, -11.64051170696115456 ) ) ;
#14005 = CARTESIAN_POINT ( 'NONE',  ( -35.00000000000000000, 65.00000000000000000, -26.49999999999998934 ) ) ;
#14006 = PRODUCT_DEFINITION_SHAPE ( 'NONE', 'NONE',  #16891 ) ;
#14007 = CARTESIAN_POINT ( 'NONE',  ( -12.69436033797397201, 18.86475830428287992, 12.05735700452609471 ) ) ;
#14008 = B_SPLINE_CURVE_WITH_KNOTS ( 'NONE', 3,
 ( #13118, #20200, #13748, #4092 ),
 .UNSPECIFIED., .F., .F.,
 ( 4, 4 ),
 ( 2.122554329650694460E-07, 0.0005857006111726079448 ),
 .UNSPECIFIED. ) ;
#14009 = LINE ( 'NONE', #12829, #18011 ) ;
#14010 = CARTESIAN_POINT ( 'NONE',  ( 190.9472490432335690, 16.27581557030192982, -22.03054070023845767 ) ) ;
#14011 = DIRECTION ( 'NONE',  ( 0.000000000000000000, 0.000000000000000000, -1.000000000000000000 ) ) ;
#14012 = VECTOR ( 'NONE', #230, 1000.000000000000227 ) ;
#14013 = ORIENTED_EDGE ( 'NONE', *, *, #19632, .F. ) ;
#14014 = CARTESIAN_POINT ( 'NONE',  ( 4.000000000000000000, 1.759474945355379960, -3.047500000000001652 ) ) ;
#14015 = DIRECTION ( 'NONE',  ( 0.000000000000000000, 0.9718000864392480898, -0.2358062594518430810 ) ) ;
#14016 = FACE_OUTER_BOUND ( 'NONE', #9486, .T. ) ;
#14017 = ORIENTED_EDGE ( 'NONE', *, *, #7090, .F. ) ;
#14018 = CARTESIAN_POINT ( 'NONE',  ( 80.76021944741209779, 65.35629346140643747, 0.4967719932253782389 ) ) ;
#14019 = VERTEX_POINT ( 'NONE', #3488 ) ;
#14020 = EDGE_LOOP ( 'NONE', ( #11417, #2777 ) ) ;
#14021 = CARTESIAN_POINT ( 'NONE',  ( -3.195128392259165118, 69.93605911897348903, 1.714708221107726471 ) ) ;
#14022 = CARTESIAN_POINT ( 'NONE',  ( 221.7323030100353662, 32.17036527648973276, -14.00000000000005507 ) ) ;
#14023 = EDGE_CURVE ( 'NONE', #270, #11709, #9934, .T. ) ;
#14024 = APPLICATION_PROTOCOL_DEFINITION ( 'draft international standard', 'automotive_design', 1998, #3237 ) ;
#14025 = AXIS2_PLACEMENT_3D ( 'NONE', #219, #5076, #14974 ) ;
#14026 = VECTOR ( 'NONE', #1179, 1000.000000000000114 ) ;
#14027 = CARTESIAN_POINT ( 'NONE',  ( 208.1960812450810465, 4.072754371081482638, -2.187257959407754804 ) ) ;
#14028 = ORIENTED_EDGE ( 'NONE', *, *, #2799, .T. ) ;
#14029 = DIRECTION ( 'NONE',  ( 0.8660254037844358210, 0.5000000000000047740, 0.000000000000000000 ) ) ;
#14030 = ORIENTED_EDGE ( 'NONE', *, *, #4622, .T. ) ;
#14031 = DIRECTION ( 'NONE',  ( 0.5000000000000007772, -0.8660254037844381525, 0.000000000000000000 ) ) ;
#14032 = DIRECTION ( 'NONE',  ( -0.2300325188655826802, 0.3984280100682314751, 0.8878852184023702243 ) ) ;
#14033 = DIRECTION ( 'NONE',  ( -0.8660254037844357100, -0.5000000000000051070, 0.000000000000000000 ) ) ;
#14034 = FACE_OUTER_BOUND ( 'NONE', #2151, .T. ) ;
#14035 = ADVANCED_FACE ( 'NONE', ( #6866 ), #14791, .T. ) ;
#14036 = DIRECTION ( 'NONE',  ( -0.8660254037844361541, -0.5000000000000045519, -4.336808689942050770E-16 ) ) ;
#14037 = DIRECTION ( 'NONE',  ( 0.8660254037844352659, 0.5000000000000056621, 0.000000000000000000 ) ) ;
#14038 = CARTESIAN_POINT ( 'NONE',  ( 0.000000000000000000, -4.685197434473809430, 6.071532165918824830E-15 ) ) ;
#14039 = ORIENTED_EDGE ( 'NONE', *, *, #14124, .F. ) ;
#14040 = VECTOR ( 'NONE', #9408, 1000.000000000000227 ) ;
#14041 = CARTESIAN_POINT ( 'NONE',  ( 212.7675431533135679, 7.484909225033065994, -2.551678190571531335 ) ) ;
#14042 = CARTESIAN_POINT ( 'NONE',  ( -3.905172448840461108, 75.66345017797092964, 3.167069675338881396 ) ) ;
#14043 = CYLINDRICAL_SURFACE ( 'NONE', #18679, 12.47473710546057646 ) ;
#14044 = DIRECTION ( 'NONE',  ( 0.8660254037844361541, 0.5000000000000043299, 0.000000000000000000 ) ) ;
#14045 = EDGE_CURVE ( 'NONE', #3287, #19907, #10031, .T. ) ;
#14047 = ORIENTED_EDGE ( 'NONE', *, *, #3122, .F. ) ;
#14046 = ORIENTED_EDGE ( 'NONE', *, *, #2816, .F. ) ;
#14048 = EDGE_CURVE ( 'NONE', #9189, #4229, #2586, .T. ) ;
#14049 = CARTESIAN_POINT ( 'NONE',  ( 5.000000000000004441, -2.342598717236899830, 4.057500000000059615 ) ) ;
#14050 = CARTESIAN_POINT ( 'NONE',  ( 197.7441788599589074, -1.188834193869147571, -15.43274561385865873 ) ) ;
#14051 = EDGE_LOOP ( 'NONE', ( #16695, #7281, #3406, #15036, #13879 ) ) ;
#14052 = UNCERTAINTY_MEASURE_WITH_UNIT (LENGTH_MEASURE( 1.000000000000000082E-05 ), #5433, 'distance_accuracy_value', 'NONE');
#14053 = B_SPLINE_CURVE_WITH_KNOTS ( 'NONE', 3,
 ( #20451, #1174, #7623, #7725 ),
 .UNSPECIFIED., .F., .F.,
 ( 4, 4 ),
 ( 3.577803810398533474E-07, 0.0006730085724280226306 ),
 .UNSPECIFIED. ) ;
#14054 = CARTESIAN_POINT ( 'NONE',  ( 229.1737920261087709, 37.77475107125530229, -11.32356490392481696 ) ) ;
#14055 = DIRECTION ( 'NONE',  ( 0.000000000000000000, 0.000000000000000000, 1.000000000000000000 ) ) ;
#14056 = CIRCLE ( 'NONE', #12700, 11.98469917212512215 ) ;
#14057 = FACE_OUTER_BOUND ( 'NONE', #4061, .T. ) ;
#14058 = LINE ( 'NONE', #15655, #7510 ) ;
#14059 = ORIENTED_EDGE ( 'NONE', *, *, #14328, .T. ) ;
#14060 = DIRECTION ( 'NONE',  ( 0.000000000000000000, 0.000000000000000000, 1.000000000000000000 ) ) ;
#14061 = DIRECTION ( 'NONE',  ( 0.000000000000000000, 0.000000000000000000, -1.000000000000000000 ) ) ;
#14062 = CYLINDRICAL_SURFACE ( 'NONE', #2974, 12.47473710546057646 ) ;
#14063 = EDGE_CURVE ( 'NONE', #16111, #3757, #19180, .T. ) ;
#14064 = LINE ( 'NONE', #2509, #4480 ) ;
#14065 = PLANE ( 'NONE',  #6426 ) ;
#14066 = B_SPLINE_CURVE_WITH_KNOTS ( 'NONE', 3,
 ( #2842, #1559, #8103, #4836 ),
 .UNSPECIFIED., .F., .F.,
 ( 4, 4 ),
 ( 5.847970035487016200E-07, 0.0005665110192881506234 ),
 .UNSPECIFIED. ) ;
#14068 = VERTEX_POINT ( 'NONE', #3898 ) ;
#14067 = ORIENTED_EDGE ( 'NONE', *, *, #2660, .F. ) ;
#14069 = ORIENTED_EDGE ( 'NONE', *, *, #15528, .F. ) ;
#14070 = FACE_BOUND ( 'NONE', #16708, .T. ) ;
#14071 = EDGE_CURVE ( 'NONE', #15363, #15277, #7980, .T. ) ;
#14072 = ORIENTED_EDGE ( 'NONE', *, *, #18084, .F. ) ;
#14073 = ORIENTED_EDGE ( 'NONE', *, *, #7695, .T. ) ;
#14074 = AXIS2_PLACEMENT_3D ( 'NONE', #5037, #16714, #11514 ) ;
#14075 = CARTESIAN_POINT ( 'NONE',  ( 207.0325450024345457, 14.94799179197019789, -1.381056684022670344 ) ) ;
#14076 = CARTESIAN_POINT ( 'NONE',  ( 207.3877668936371492, 11.02908132907535332, -2.195132782454303655 ) ) ;
#14077 = CARTESIAN_POINT ( 'NONE',  ( 208.3673372177917429, 15.71863443681889549, -1.942038651984890674 ) ) ;
#14078 = EDGE_CURVE ( 'NONE', #19163, #1466, #3931, .T. ) ;
#14079 = DIRECTION ( 'NONE',  ( 0.5000000000000051070, -0.8660254037844359321, 0.000000000000000000 ) ) ;
#14080 = CARTESIAN_POINT ( 'NONE',  ( 26.00000000000000355, 0.000000000000000000, 0.000000000000000000 ) ) ;
#14081 = EDGE_CURVE ( 'NONE', #18781, #20638, #213, .T. ) ;
#14082 = ORIENTED_EDGE ( 'NONE', *, *, #17147, .F. ) ;
#14083 = EDGE_CURVE ( 'NONE', #14800, #2300, #10352, .T. ) ;
#14084 = DIRECTION ( 'NONE',  ( 0.000000000000000000, 0.000000000000000000, -1.000000000000000000 ) ) ;
#14085 = AXIS2_PLACEMENT_3D ( 'NONE', #9847, #8368, #9945 ) ;
#14086 = DIRECTION ( 'NONE',  ( -0.5943026915289658652, -0.3431208189343721848, -0.7273736415730450711 ) ) ;
#14087 = CARTESIAN_POINT ( 'NONE',  ( -28.21861819285526352, 49.99051376660081303, -12.54928731108197404 ) ) ;
#14088 = DIRECTION ( 'NONE',  ( 0.8660254037844355990, 0.5000000000000054401, 0.000000000000000000 ) ) ;
#14089 = AXIS2_PLACEMENT_3D ( 'NONE', #17831, #6457, #16343 ) ;
#14090 = EDGE_CURVE ( 'NONE', #19247, #11249, #15171, .T. ) ;
#14091 = DIRECTION ( 'NONE',  ( 0.8660254037844370423, 0.5000000000000026645, -0.000000000000000000 ) ) ;
#14092 = CARTESIAN_POINT ( 'NONE',  ( -27.87663165302654633, 46.26680992104923718, -3.912879880524708920 ) ) ;
#14094 = ORIENTED_EDGE ( 'NONE', *, *, #14998, .T. ) ;
#14093 = VERTEX_POINT ( 'NONE', #8566 ) ;
#14095 = CARTESIAN_POINT ( 'NONE',  ( 195.4946457851292507, 4.162584655573419390, -16.75125533358848884 ) ) ;
#14096 = APPLICATION_CONTEXT ( 'automotive_design' ) ;
#14097 = LINE ( 'NONE', #13991, #15295 ) ;
#14098 = CARTESIAN_POINT ( 'NONE',  ( 1.501123442541940634, 76.50873768552941101, -2.871813542384042961 ) ) ;
#14099 = ORIENTED_EDGE ( 'NONE', *, *, #15224, .F. ) ;
#14100 = ORIENTED_EDGE ( 'NONE', *, *, #12286, .T. ) ;
#14101 = CYLINDRICAL_SURFACE ( 'NONE', #10530, 13.99999999999999822 ) ;
#14102 = CARTESIAN_POINT ( 'NONE',  ( 228.6672469504414664, 37.67264698757139030, -10.82724490084735791 ) ) ;
#14103 = CARTESIAN_POINT ( 'NONE',  ( -33.51303128878281257, 52.95196417805331635, -3.530639089860408308 ) ) ;
#14104 = AXIS2_PLACEMENT_3D ( 'NONE', #11298, #8092, #15984 ) ;
#14105 = CARTESIAN_POINT ( 'NONE',  ( -28.06703991579542645, 9.091582454895631216, 3.326663291586896776 ) ) ;
#14106 = EDGE_CURVE ( 'NONE', #11719, #4766, #16133, .T. ) ;
#14107 = ORIENTED_EDGE ( 'NONE', *, *, #17317, .T. ) ;
#14108 = ORIENTED_EDGE ( 'NONE', *, *, #14345, .T. ) ;
#14109 = AXIS2_PLACEMENT_3D ( 'NONE', #16639, #15075, #20127 ) ;
#14110 = CARTESIAN_POINT ( 'NONE',  ( 219.4425538016219832, 36.34917468585137357, -17.48404651990730940 ) ) ;
#14111 = ORIENTED_EDGE ( 'NONE', *, *, #13502, .T. ) ;
#14112 = AXIS2_PLACEMENT_3D ( 'NONE', #6645, #5064, #15579 ) ;
#14113 = EDGE_CURVE ( 'NONE', #2143, #18516, #8993, .T. ) ;
#14114 =( LENGTH_UNIT ( ) NAMED_UNIT ( * ) SI_UNIT ( .MILLI., .METRE. ) );
#14115 = LINE ( 'NONE', #15904, #3515 ) ;
#14116 = ADVANCED_FACE ( 'NONE', ( #11862 ), #16839, .T. ) ;
#14117 = CYLINDRICAL_SURFACE ( 'NONE', #3347, 3.902363844300889451 ) ;
#14118 = CARTESIAN_POINT ( 'NONE',  ( 80.60041742765380945, 65.51180379921632380, -25.49148684086367211 ) ) ;
#14119 = EDGE_CURVE ( 'NONE', #14158, #15392, #5478, .T. ) ;
#14120 = DIRECTION ( 'NONE',  ( 0.4999999999999995004, -0.8660254037844390407, 0.000000000000000000 ) ) ;
#14121 = LINE ( 'NONE', #15810, #4658 ) ;
#14122 = DIRECTION ( 'NONE',  ( 0.8660254037844380415, 0.5000000000000014433, 0.000000000000000000 ) ) ;
#14123 = VECTOR ( 'NONE', #9962, 1000.000000000000114 ) ;
#14124 = EDGE_CURVE ( 'NONE', #14385, #10039, #5371, .T. ) ;
#14125 = CARTESIAN_POINT ( 'NONE',  ( -15.99999999999999289, 80.00000000000000000, 0.000000000000000000 ) ) ;
#14126 = LINE ( 'NONE', #9211, #9588 ) ;
#14127 = LINE ( 'NONE', #9007, #10907 ) ;
#14128 = VECTOR ( 'NONE', #2728, 1000.000000000000000 ) ;
#14129 = ORIENTED_EDGE ( 'NONE', *, *, #8083, .F. ) ;
#14130 = CARTESIAN_POINT ( 'NONE',  ( 79.87047281314329439, 67.12885141646589204, 0.3411143157775017309 ) ) ;
#14131 = VERTEX_POINT ( 'NONE', #3794 ) ;
#14132 = ORIENTED_EDGE ( 'NONE', *, *, #13702, .T. ) ;
#14133 = CARTESIAN_POINT ( 'NONE',  ( -3.510843195177425713, 80.00000000000000000, 0.5205403966592461185 ) ) ;
#14134 = DIRECTION ( 'NONE',  ( -1.000000000000000000, -0.000000000000000000, -0.000000000000000000 ) ) ;
#14135 = ADVANCED_FACE ( 'NONE', ( #10245 ), #16736, .F. ) ;
#14136 = SHAPE_REPRESENTATION ( 'Pin', ( #18233 ), #7378 ) ;
#14137 = APPLICATION_PROTOCOL_DEFINITION ( 'draft international standard', 'automotive_design', 1998, #18541 ) ;
#14138 = CARTESIAN_POINT ( 'NONE',  ( 1.500000000000001332, 9.797174393178825657E-16, -8.000000000000000000 ) ) ;
#14139 = ORIENTED_EDGE ( 'NONE', *, *, #18992, .T. ) ;
#14140 = VECTOR ( 'NONE', #19349, 1000.000000000000227 ) ;
#14141 = CARTESIAN_POINT ( 'NONE',  ( 202.2312820113153862, 1.144182166681870561, -23.86786078788932741 ) ) ;
#14142 = LINE ( 'NONE', #7538, #15876 ) ;
#14143 = CARTESIAN_POINT ( 'NONE',  ( 226.6453546267926527, 41.17466721956452602, -10.52303454827235996 ) ) ;
#14144 = DIRECTION ( 'NONE',  ( 0.8660254037844359321, 0.5000000000000046629, 0.000000000000000000 ) ) ;
#14145 = CARTESIAN_POINT ( 'NONE',  ( 226.6211368133091923, 39.11482588413117867, -14.00000000000005507 ) ) ;
#14146 = CARTESIAN_POINT ( 'NONE',  ( 216.3417993343409194, 15.66764510725598214, -11.13829696442610029 ) ) ;
#14147 = DIRECTION ( 'NONE',  ( -0.5000000000000051070, 0.8660254037844359321, -0.000000000000000000 ) ) ;
#14148 = EDGE_CURVE ( 'NONE', #13052, #8243, #19489, .T. ) ;
#14149 = CARTESIAN_POINT ( 'NONE',  ( 26.99999999999999645, 65.00000000000000000, -12.50000000000000000 ) ) ;
#14150 = VERTEX_POINT ( 'NONE', #5896 ) ;
#14151 = CARTESIAN_POINT ( 'NONE',  ( -14.99999999999999645, 0.000000000000000000, -15.00000000000000000 ) ) ;
#14152 = CARTESIAN_POINT ( 'NONE',  ( -4.674616544174982735, 67.03307707865302234, 5.290582662559626392 ) ) ;
#14153 = VECTOR ( 'NONE', #14640, 1000.000000000000114 ) ;
#14154 = B_SPLINE_CURVE_WITH_KNOTS ( 'NONE', 3,
 ( #17201, #6050, #2687, #9027 ),
 .UNSPECIFIED., .F., .F.,
 ( 4, 4 ),
 ( 4.351832736271508415E-07, 0.0005663614055661156648 ),
 .UNSPECIFIED. ) ;
#14155 = DIRECTION ( 'NONE',  ( -0.6958540455341998276, 0.000000000000000000, -0.7181832268395633712 ) ) ;
#14156 = CARTESIAN_POINT ( 'NONE',  ( 227.5312376355471145, 39.64027283883993391, -14.00000000000005507 ) ) ;
#14157 = VECTOR ( 'NONE', #7573, 1000.000000000000227 ) ;
#14159 = ORIENTED_EDGE ( 'NONE', *, *, #3165, .F. ) ;
#14158 = VERTEX_POINT ( 'NONE', #17367 ) ;
#14160 = CARTESIAN_POINT ( 'NONE',  ( 222.0128931678030710, 32.30914647947069795, -12.46964089162990952 ) ) ;
#14161 = DIRECTION ( 'NONE',  ( 0.000000000000000000, 0.000000000000000000, 1.000000000000000000 ) ) ;
#14162 = ORIENTED_EDGE ( 'NONE', *, *, #19061, .T. ) ;
#14163 = EDGE_CURVE ( 'NONE', #6373, #3452, #15379, .T. ) ;
#14164 = CARTESIAN_POINT ( 'NONE',  ( 66.35003277998524140, 79.49709411292175787, -21.83015642861430550 ) ) ;
#14165 = CARTESIAN_POINT ( 'NONE',  ( 43.00000000000000000, 0.000000000000000000, 3.309499999999999886 ) ) ;
#14166 = DIRECTION ( 'NONE',  ( -0.8660254037844355990, -0.5000000000000054401, -1.779954182985030830E-14 ) ) ;
#14167=STYLED_ITEM('',(#20995),#17281);
#14168 = CARTESIAN_POINT ( 'NONE',  ( 229.4107422034203978, 37.03787224932305122, -15.89588733938011167 ) ) ;
#14169 = VECTOR ( 'NONE', #20855, 1000.000000000000227 ) ;
#14170 = ORIENTED_EDGE ( 'NONE', *, *, #2940, .T. ) ;
#14171 = DIRECTION ( 'NONE',  ( 0.8660254037844364872, 0.5000000000000041078, -0.000000000000000000 ) ) ;
#14172 = EDGE_CURVE ( 'NONE', #17905, #13143, #18158, .T. ) ;
#14173 = CARTESIAN_POINT ( 'NONE',  ( 225.6000782901530215, 42.98513894257393986, -14.55761806292083982 ) ) ;
#14174 = B_SPLINE_CURVE_WITH_KNOTS ( 'NONE', 3,
 ( #16697, #10203, #14810, #19757 ),
 .UNSPECIFIED., .F., .F.,
 ( 4, 4 ),
 ( 2.739126000505470127E-07, 0.0004523271543799366580 ),
 .UNSPECIFIED. ) ;
#14175 = FACE_OUTER_BOUND ( 'NONE', #5000, .T. ) ;
#14176 = CARTESIAN_POINT ( 'NONE',  ( 197.9670180026625417, -1.060177954843255499, -16.89203719259486647 ) ) ;
#14178 = ORIENTED_EDGE ( 'NONE', *, *, #3201, .F. ) ;
#14177 = ORIENTED_EDGE ( 'NONE', *, *, #6646, .T. ) ;
#14179 = ORIENTED_EDGE ( 'NONE', *, *, #16664, .F. ) ;
#14180 = FACE_BOUND ( 'NONE', #14020, .T. ) ;
#14181 = EDGE_LOOP ( 'NONE', ( #3762, #2462, #10754, #19168, #14341, #6195, #5170, #13040, #4884, #11187, #18850, #15344 ) ) ;
#14182 = ORIENTED_EDGE ( 'NONE', *, *, #14461, .F. ) ;
#14183 = VECTOR ( 'NONE', #10718, 1000.000000000000000 ) ;
#14184 = CARTESIAN_POINT ( 'NONE',  ( -18.51922807846269592, 10.76830012676478709, 12.24661932923539354 ) ) ;
#14185 = VECTOR ( 'NONE', #858, 1000.000000000000114 ) ;
#14186 = DIRECTION ( 'NONE',  ( -0.8660254037844360431, -0.5000000000000046629, 0.000000000000000000 ) ) ;
#14187 = CARTESIAN_POINT ( 'NONE',  ( -15.99999999999999289, 80.00000000000000000, 0.000000000000000000 ) ) ;
#14188 =( GEOMETRIC_REPRESENTATION_CONTEXT ( 3 ) GLOBAL_UNCERTAINTY_ASSIGNED_CONTEXT ( ( #14052 ) ) GLOBAL_UNIT_ASSIGNED_CONTEXT ( ( #5433, #10098, #18500 ) ) REPRESENTATION_CONTEXT ( 'NONE', 'WORKASPACE' ) );
#14189 = CARTESIAN_POINT ( 'NONE',  ( 209.8373868153248623, 12.26636014609055891, -2.844109184787622535 ) ) ;
#14190 = PRODUCT_RELATED_PRODUCT_CATEGORY ( 'part', '', ( #18380 ) ) ;
#14191 = PLANE ( 'NONE',  #12119 ) ;
#14192 = ORIENTED_EDGE ( 'NONE', *, *, #20416, .T. ) ;
#14193 = CARTESIAN_POINT ( 'NONE',  ( 227.9553588074475670, 39.88513931160575510, -14.00000000000005507 ) ) ;
#14194 = ADVANCED_FACE ( 'NONE', ( #10572 ), #8977, .F. ) ;
#14195 = AXIS2_PLACEMENT_3D ( 'NONE', #8726, #15223, #5738 ) ;
#14196 = EDGE_CURVE ( 'NONE', #14800, #16971, #10686, .T. ) ;
#14197 = CARTESIAN_POINT ( 'NONE',  ( 211.0762420533076806, 12.80459687405399549, -3.334988897836945743 ) ) ;
#14198 = CARTESIAN_POINT ( 'NONE',  ( -7.283141699791834789, 49.98730520602950378, -8.963927540845297415 ) ) ;
#14199 = DIRECTION ( 'NONE',  ( 0.5000000000000054401, -0.8660254037844354880, 0.000000000000000000 ) ) ;
#14200 = DIRECTION ( 'NONE',  ( -0.06808332454812728030, 0.1179237772655570421, 0.9906859460363297565 ) ) ;
#14201 = CARTESIAN_POINT ( 'NONE',  ( 5.000000000000004441, 4.685197434473814759, -6.938893903907228378E-15 ) ) ;
#14203 = ORIENTED_EDGE ( 'NONE', *, *, #4632, .T. ) ;
#14202 = ORIENTED_EDGE ( 'NONE', *, *, #576, .F. ) ;
#14204 = ORIENTED_EDGE ( 'NONE', *, *, #1376, .F. ) ;
#14205 = PLANE ( 'NONE',  #13584 ) ;
#14206 = PLANE ( 'NONE',  #7459 ) ;
#14207 = CARTESIAN_POINT ( 'NONE',  ( -3.599723856067730487, 79.99999999992392929, -1.584264587336005503 ) ) ;
#14208 = EDGE_LOOP ( 'NONE', ( #92, #17986, #8983, #2489, #13799, #16917, #2838, #5901, #7217, #3365, #10807, #17089 ) ) ;
#14209 = ORIENTED_EDGE ( 'NONE', *, *, #873, .F. ) ;
#14210 = EDGE_CURVE ( 'NONE', #8547, #11638, #13768, .T. ) ;
#14211 = ORIENTED_EDGE ( 'NONE', *, *, #5437, .T. ) ;
#14212 = CARTESIAN_POINT ( 'NONE',  ( 46.51452848080092650, 183.3908428320656299, 11.00000000000001066 ) ) ;
#14213 = DIRECTION ( 'NONE',  ( 0.5000000000000049960, -0.8660254037844357100, 0.000000000000000000 ) ) ;
#14214 = CARTESIAN_POINT ( 'NONE',  ( 1.503428104146816491, 53.42452153058392383, -2.951951819453562997 ) ) ;
#14215 = CARTESIAN_POINT ( 'NONE',  ( -34.33329038210762718, 65.74999999999997158, -2.193932927905878127 ) ) ;
#14216 = VERTEX_POINT ( 'NONE', #9079 ) ;
#14217 = VECTOR ( 'NONE', #8130, 1000.000000000000227 ) ;
#14218 = ORIENTED_EDGE ( 'NONE', *, *, #16335, .T. ) ;
#14219 = CARTESIAN_POINT ( 'NONE',  ( 5.000000000000000000, -2.342598717236899386, 4.057500000000001883 ) ) ;
#14220 = EDGE_CURVE ( 'NONE', #2011, #10374, #20216, .T. ) ;
#14221 = DIRECTION ( 'NONE',  ( -0.5000000000000049960, 0.8660254037844358210, -0.000000000000000000 ) ) ;
#14222 = CARTESIAN_POINT ( 'NONE',  ( 58.37797649651341203, 276.8427481158987007, -28.99999999999998934 ) ) ;
#14223 = FACE_OUTER_BOUND ( 'NONE', #9556, .T. ) ;
#14224 = ADVANCED_FACE ( 'NONE', ( #1043 ), #12491, .F. ) ;
#14225 = LINE ( 'NONE', #2661, #2445 ) ;
#14226 = DIRECTION ( 'NONE',  ( -0.000000000000000000, -1.000000000000000000, 1.302777330458572662E-15 ) ) ;
#14227 = DIRECTION ( 'NONE',  ( 0.4586056507527268566, -0.7943282877419068910, 0.3984010898462484462 ) ) ;
#14228 = VERTEX_POINT ( 'NONE', #4323 ) ;
#14229 = LINE ( 'NONE', #12832, #6021 ) ;
#14230 = CARTESIAN_POINT ( 'NONE',  ( 215.6527207509367088, 8.377847197037317173, -3.480441514389753799 ) ) ;
#14231 = CARTESIAN_POINT ( 'NONE',  ( 226.1897974575875310, 41.96371538238017251, -16.83383072344315678 ) ) ;
#14232 = CIRCLE ( 'NONE', #10806, 17.50000000000000000 ) ;
#14233 = ORIENTED_EDGE ( 'NONE', *, *, #19751, .F. ) ;
#14234 = CARTESIAN_POINT ( 'NONE',  ( 80.65040410709035257, 67.47975763685462880, 0.5668321014029960025 ) ) ;
#14235 = ADVANCED_FACE ( 'NONE', ( #18849 ), #7496, .F. ) ;
#14236 = ORIENTED_EDGE ( 'NONE', *, *, #2843, .T. ) ;
#14237 = EDGE_CURVE ( 'NONE', #3665, #17033, #15689, .T. ) ;
#14238 = ORIENTED_EDGE ( 'NONE', *, *, #2837, .T. ) ;
#14239 = CARTESIAN_POINT ( 'NONE',  ( -3.082880228654353072, 72.10661837392622431, 0.7232648427671327651 ) ) ;
#14240 = CIRCLE ( 'NONE', #19615, 11.98469917212512215 ) ;
#14241 = ITEM_DEFINED_TRANSFORMATION ( 'NONE', 'NONE', #20255,  #18233 ) ;
#14242 = B_SPLINE_CURVE_WITH_KNOTS ( 'NONE', 3,
 ( #19648, #5125, #13728, #2381 ),
 .UNSPECIFIED., .F., .F.,
 ( 4, 4 ),
 ( 5.538124335884803249E-06, 0.0008595238623188111412 ),
 .UNSPECIFIED. ) ;
#14243 = EDGE_CURVE ( 'NONE', #9665, #5157, #20629, .T. ) ;
#14244 = DIRECTION ( 'NONE',  ( 0.8660254037844354880, 0.5000000000000053291, 0.000000000000000000 ) ) ;
#14245 = ORIENTED_EDGE ( 'NONE', *, *, #10706, .F. ) ;
#14246 = CARTESIAN_POINT ( 'NONE',  ( 1.500000000000001332, 7.509176090703883811E-16, -6.500000000000047962 ) ) ;
#14247 = VECTOR ( 'NONE', #1130, 1000.000000000000114 ) ;
#14248 = CARTESIAN_POINT ( 'NONE',  ( 0.000000000000000000, 4.685197434473812983, -6.938893903907228378E-15 ) ) ;
#14249 = CARTESIAN_POINT ( 'NONE',  ( 209.4061049964370227, 30.62402206602542165, -16.16870873105882112 ) ) ;
#14250 = LINE ( 'NONE', #12335, #8823 ) ;
#14251 = VECTOR ( 'NONE', #1459, 1000.000000000000114 ) ;
#14252 = EDGE_LOOP ( 'NONE', ( #326, #12241, #20875 ) ) ;
#14253 = DIRECTION ( 'NONE',  ( -0.5000000000000034417, 0.8660254037844364872, 0.000000000000000000 ) ) ;
#14254 = CYLINDRICAL_SURFACE ( 'NONE', #7524, 12.47473710546057646 ) ;
#14255 = EDGE_CURVE ( 'NONE', #1224, #12038, #7805, .T. ) ;
#14256 = DIRECTION ( 'NONE',  ( -0.8660254037844355990, -0.5000000000000051070, -2.294936594593527877E-16 ) ) ;
#14257 = CARTESIAN_POINT ( 'NONE',  ( 209.8762589913676777, 12.46581291157635540, -14.99881147502670586 ) ) ;
#14258 = DIRECTION ( 'NONE',  ( 0.000000000000000000, 0.000000000000000000, -1.000000000000000000 ) ) ;
#14259 = ORIENTED_EDGE ( 'NONE', *, *, #1986, .T. ) ;
#14260 = DIRECTION ( 'NONE',  ( 0.5000000000000041078, -0.8660254037844362651, 0.000000000000000000 ) ) ;
#14261 = CARTESIAN_POINT ( 'NONE',  ( -3.836925286482116171, 76.23982303504118363, 2.898234736985788818 ) ) ;
#14262 = CARTESIAN_POINT ( 'NONE',  ( 195.0522846737218288, 8.031185266226035679, -5.585956497639847029 ) ) ;
#14263 = FACE_OUTER_BOUND ( 'NONE', #1674, .T. ) ;
#14264 = CARTESIAN_POINT ( 'NONE',  ( -33.48481952675158624, 76.25000000000001421, -2.578432583507807685 ) ) ;
#14266 = ORIENTED_EDGE ( 'NONE', *, *, #14586, .T. ) ;
#14265 = EDGE_LOOP ( 'NONE', ( #10958, #18545, #1335, #19151 ) ) ;
#14267 = EDGE_LOOP ( 'NONE', ( #10461, #14841, #4365 ) ) ;
#14268 = CIRCLE ( 'NONE', #12558, 6.500000000000000000 ) ;
#14269 = DIRECTION ( 'NONE',  ( -0.000000000000000000, 1.000000000000000000, 1.224646799147353207E-16 ) ) ;
#14270 = CARTESIAN_POINT ( 'NONE',  ( 16.51452848080062097, 235.3523670591319217, -8.999999999999932498 ) ) ;
#14271 = PRODUCT_DEFINITION_CONTEXT ( 'detailed design', #14096, 'design' ) ;
#14272 = VECTOR ( 'NONE', #13050, 1000.000000000000114 ) ;
#14273 = LINE ( 'NONE', #9669, #8676 ) ;
#14274 = VERTEX_POINT ( 'NONE', #17890 ) ;
#14275 = DIRECTION ( 'NONE',  ( 0.8660254037844352659, 0.5000000000000056621, 0.000000000000000000 ) ) ;
#14276 = AXIS2_PLACEMENT_3D ( 'NONE', #9949, #13371, #16657 ) ;
#14277 = AXIS2_PLACEMENT_3D ( 'NONE', #714, #19888, #16926 ) ;
#14278 = CARTESIAN_POINT ( 'NONE',  ( 0.000000000000000000, 2.342598717236899830, -4.057500000000030305 ) ) ;
#14279 = DIRECTION ( 'NONE',  ( 1.000000000000000000, 0.000000000000000000, 0.000000000000000000 ) ) ;
#14280 = VECTOR ( 'NONE', #4842, 1000.000000000000000 ) ;
#14281 = EDGE_LOOP ( 'NONE', ( #20244, #5532, #8844, #20307, #3683, #9462 ) ) ;
#14282 = DIRECTION ( 'NONE',  ( 0.000000000000000000, 0.000000000000000000, -1.000000000000000000 ) ) ;
#14283 = CARTESIAN_POINT ( 'NONE',  ( 229.4772413560592383, 37.24916141425800475, -11.55788255683066268 ) ) ;
#14284 = CONICAL_SURFACE ( 'NONE', #20684, 14.99999999999999645, 0.7853981633974543852 ) ;
#14285 = DIRECTION ( 'NONE',  ( -0.8660254037844361541, -0.5000000000000044409, 5.976026924694052093E-17 ) ) ;
#14286 = LINE ( 'NONE', #9158, #14919 ) ;
#14287 = ORIENTED_EDGE ( 'NONE', *, *, #12418, .F. ) ;
#14288 = DIRECTION ( 'NONE',  ( 1.000000000000000000, 0.000000000000000000, 0.000000000000000000 ) ) ;
#14289 = VECTOR ( 'NONE', #5543, 1000.000000000000227 ) ;
#14290 = VERTEX_POINT ( 'NONE', #9700 ) ;
#14291 = EDGE_LOOP ( 'NONE', ( #971, #11377, #12882, #18253 ) ) ;
#14292 = PLANE ( 'NONE',  #16303 ) ;
#14293 = CARTESIAN_POINT ( 'NONE',  ( 30.10683012259193703, -10.00000000000000000, 0.000000000000000000 ) ) ;
#14294 = CARTESIAN_POINT ( 'NONE',  ( 221.7578608766766308, 32.54489729930224939, -15.94147978600234872 ) ) ;
#14295 = VECTOR ( 'NONE', #20387, 1000.000000000000227 ) ;
#14296 = AXIS2_PLACEMENT_3D ( 'NONE', #13403, #15430, #10298 ) ;
#14297 = DIRECTION ( 'NONE',  ( 0.8660254037844355990, 0.5000000000000054401, 4.449885457462577074E-15 ) ) ;
#14298 = EDGE_CURVE ( 'NONE', #12209, #11821, #15884, .T. ) ;
#14299 = CARTESIAN_POINT ( 'NONE',  ( 214.4612834781239314, 14.93596812906266180, -20.67833249884127866 ) ) ;
#14300 = ORIENTED_EDGE ( 'NONE', *, *, #11000, .T. ) ;
#14301 = CARTESIAN_POINT ( 'NONE',  ( 211.8034485311565049, 13.57847631115287435, -23.60546391700164648 ) ) ;
#14302 = CARTESIAN_POINT ( 'NONE',  ( 199.2144802262915846, 21.04890371929339921, -14.00000000000005507 ) ) ;
#14303 = CARTESIAN_POINT ( 'NONE',  ( -4.526739825310654552, 50.00778237576246710, -13.04232340071289897 ) ) ;
#14304 = CARTESIAN_POINT ( 'NONE',  ( 94.31531706421118599, 208.0571376747316492, 11.00000000000001066 ) ) ;
#14305 = LINE ( 'NONE', #2844, #8 ) ;
#14306 = EDGE_CURVE ( 'NONE', #11555, #13220, #6466, .T. ) ;
#14307 = CARTESIAN_POINT ( 'NONE',  ( 97.85954905003006843, 199.4060149184856243, 13.16759434796133554 ) ) ;
#14309 = ORIENTED_EDGE ( 'NONE', *, *, #14555, .T. ) ;
#14308 = VERTEX_POINT ( 'NONE', #8106 ) ;
#14310 = DIRECTION ( 'NONE',  ( 1.000000000000000000, -0.000000000000000000, -0.000000000000000000 ) ) ;
#14311 = DIRECTION ( 'NONE',  ( 0.9987303135603810000, 0.000000000000000000, 0.05037619254750287656 ) ) ;
#14312 = LINE ( 'NONE', #2953, #2316 ) ;
#14313 = ORIENTED_EDGE ( 'NONE', *, *, #19380, .F. ) ;
#14314 = ORIENTED_EDGE ( 'NONE', *, *, #9374, .T. ) ;
#14315 = ORIENTED_EDGE ( 'NONE', *, *, #4847, .T. ) ;
#14316 = DIRECTION ( 'NONE',  ( -0.5000000000000163203, -0.8660254037844291597, 1.060575238724920473E-16 ) ) ;
#14317 = LINE ( 'NONE', #11113, #20666 ) ;
#14318 = CARTESIAN_POINT ( 'NONE',  ( -0.09406327930139435356, 50.50908616029219900, -8.609884709595448271 ) ) ;
#14319 = FACE_OUTER_BOUND ( 'NONE', #15007, .T. ) ;
#14320 = ORIENTED_EDGE ( 'NONE', *, *, #20771, .T. ) ;
#14321 = EDGE_CURVE ( 'NONE', #16948, #3183, #11380, .T. ) ;
#14322 = EDGE_LOOP ( 'NONE', ( #14030, #6876, #601, #1702 ) ) ;
#14323 = EDGE_CURVE ( 'NONE', #13637, #7692, #15997, .T. ) ;
#14324 = CARTESIAN_POINT ( 'NONE',  ( -0.1607576869230442629, 66.25779166050591584, 2.455816886943473332 ) ) ;
#14325 = AXIS2_PLACEMENT_3D ( 'NONE', #18240, #3505, #15088 ) ;
#14326 = VECTOR ( 'NONE', #16623, 1000.000000000000114 ) ;
#14327 = DIRECTION ( 'NONE',  ( 0.3430151393149034611, 0.1980398830195791438, -0.9182161068802751069 ) ) ;
#14328 = EDGE_CURVE ( 'NONE', #8377, #6716, #414, .T. ) ;
#14329 = CARTESIAN_POINT ( 'NONE',  ( 228.9842339441690342, 37.45011616765739149, -16.76050993469859662 ) ) ;
#14330 = CARTESIAN_POINT ( 'NONE',  ( 226.6211368133091923, 39.11482588413117867, -14.00000000000005507 ) ) ;
#14331 = CARTESIAN_POINT ( 'NONE',  ( 72.24503483210654053, 70.17032258213592399, -24.43510331009084524 ) ) ;
#14332 = ORIENTED_EDGE ( 'NONE', *, *, #1024, .F. ) ;
#14333 = DIRECTION ( 'NONE',  ( -0.000000000000000000, 1.000000000000000000, -0.000000000000000000 ) ) ;
#14334 = CARTESIAN_POINT ( 'NONE',  ( 184.9952905943349606, 3.535126980567709687, -6.000000000000009770 ) ) ;
#14335 = DIRECTION ( 'NONE',  ( -0.8660254037844368202, -0.5000000000000031086, 0.000000000000000000 ) ) ;
#14336 = VERTEX_POINT ( 'NONE', #15786 ) ;
#14337 = VECTOR ( 'NONE', #6966, 1000.000000000000114 ) ;
#14339 = EDGE_CURVE ( 'NONE', #3730, #14650, #19265, .T. ) ;
#14338 = CARTESIAN_POINT ( 'NONE',  ( 81.70593518416212930, 63.65981237297968676, 0.4334013042838535390 ) ) ;
#14340 = CIRCLE ( 'NONE', #11606, 11.94520687646042667 ) ;
#14341 = ORIENTED_EDGE ( 'NONE', *, *, #7003, .T. ) ;
#14342 = ORIENTED_EDGE ( 'NONE', *, *, #763, .T. ) ;
#14343 = CARTESIAN_POINT ( 'NONE',  ( -0.003873131613744759151, 68.02992772322234316, 2.199708061508872881 ) ) ;
#14344 = DIRECTION ( 'NONE',  ( 0.000000000000000000, 6.938893903907178303E-18, 1.000000000000000000 ) ) ;
#14345 = EDGE_CURVE ( 'NONE', #9708, #12385, #15804, .T. ) ;
#14346 = CARTESIAN_POINT ( 'NONE',  ( 203.0246517772566506, 23.22871929987775630, -14.00000000000005507 ) ) ;
#14347 = APPLICATION_PROTOCOL_DEFINITION ( 'draft international standard', 'automotive_design', 1998, #20702 ) ;
#14348 = ADVANCED_FACE ( 'NONE', ( #13432 ), #11948, .T. ) ;
#14349 = CARTESIAN_POINT ( 'NONE',  ( 219.4034321113204555, 36.41693544113155667, -10.54376118423949826 ) ) ;
#14350 = ORIENTED_EDGE ( 'NONE', *, *, #13206, .F. ) ;
#14351 = DIRECTION ( 'NONE',  ( 0.5000000000000054401, -0.8660254037844354880, -2.081668171172167774E-16 ) ) ;
#14352 = FACE_OUTER_BOUND ( 'NONE', #12455, .T. ) ;
#14353 = VECTOR ( 'NONE', #2971, 1000.000000000000000 ) ;
#14354 = CARTESIAN_POINT ( 'NONE',  ( 208.9653092665176644, 31.66033285536642339, -14.80609056993748140 ) ) ;
#14355 = CARTESIAN_POINT ( 'NONE',  ( -15.99999999999999289, -9.999999999999994671, -4.999999999999989342 ) ) ;
#14356 = EDGE_CURVE ( 'NONE', #20547, #8036, #14926, .T. ) ;
#14357 = EDGE_CURVE ( 'NONE', #20025, #1190, #518, .T. ) ;
#14358 = EDGE_CURVE ( 'NONE', #14630, #5282, #11733, .T. ) ;
#14359 = CARTESIAN_POINT ( 'NONE',  ( 226.3972337354671538, 42.58389110082306672, -15.84136033874741756 ) ) ;
#14360 = CARTESIAN_POINT ( 'NONE',  ( 227.9553588074475954, 39.88513931160571957, -14.00000000000005507 ) ) ;
#14361 = DIRECTION ( 'NONE',  ( -1.000000000000000000, 0.000000000000000000, 0.000000000000000000 ) ) ;
#14362 = CARTESIAN_POINT ( 'NONE',  ( 192.0123155716598262, 35.38128320186126530, -9.087049258353282255 ) ) ;
#14363 = DIRECTION ( 'NONE',  ( 0.8660254037844372643, 0.5000000000000027756, -0.000000000000000000 ) ) ;
#14364 = VERTEX_POINT ( 'NONE', #16496 ) ;
#14366 = EDGE_CURVE ( 'NONE', #5956, #10193, #17102, .T. ) ;
#14365 = DIRECTION ( 'NONE',  ( -0.000000000000000000, -1.000000000000000000, -0.000000000000000000 ) ) ;
#14367 = CARTESIAN_POINT ( 'NONE',  ( 60.59842726415620717, 83.94481412498421946, -7.461880171922929961 ) ) ;
#14368 = LINE ( 'NONE', #15839, #14911 ) ;
#14369 = VECTOR ( 'NONE', #15315, 1000.000000000000227 ) ;
#14370 = CARTESIAN_POINT ( 'NONE',  ( -29.33334206987314019, 76.88745196853791697, -3.296735915519156013 ) ) ;
#14371 = VECTOR ( 'NONE', #13112, 1000.000000000000000 ) ;
#14373 = ORIENTED_EDGE ( 'NONE', *, *, #19788, .F. ) ;
#14372 = ORIENTED_EDGE ( 'NONE', *, *, #12651, .T. ) ;
#14374 = ORIENTED_EDGE ( 'NONE', *, *, #18350, .F. ) ;
#14375 = ADVANCED_FACE ( 'NONE', ( #14724 ), #7943, .F. ) ;
#14376 = CARTESIAN_POINT ( 'NONE',  ( 183.9132435853528307, 37.55142300003367950, -14.00000000000003730 ) ) ;
#14377 = EDGE_LOOP ( 'NONE', ( #1699, #12524, #16365, #19484, #18146, #2708, #10979, #10768, #9531 ) ) ;
#14378 = CARTESIAN_POINT ( 'NONE',  ( 85.37797649651368204, 230.0773763115391262, -0.9999999999999826805 ) ) ;
#14379 = CARTESIAN_POINT ( 'NONE',  ( -27.46983130148931807, 79.99999999986543742, -4.984538917065587604 ) ) ;
#14380 = CARTESIAN_POINT ( 'NONE',  ( 221.1877743307729531, 33.12044585814464881, -16.57782486433075775 ) ) ;
#14381 = EDGE_CURVE ( 'NONE', #17447, #6599, #10649, .T. ) ;
#14382 = B_SPLINE_CURVE_WITH_KNOTS ( 'NONE', 3,
 ( #617, #13555, #5160, #20006 ),
 .UNSPECIFIED., .F., .F.,
 ( 4, 4 ),
 ( 3.991550130978308204E-07, 0.0005663253773120254918 ),
 .UNSPECIFIED. ) ;
#14383 = EDGE_CURVE ( 'NONE', #8182, #13147, #6722, .T. ) ;
#14384 = DIRECTION ( 'NONE',  ( 0.000000000000000000, 0.000000000000000000, 1.000000000000000000 ) ) ;
#14385 = VERTEX_POINT ( 'NONE', #15042 ) ;
#14386 = CARTESIAN_POINT ( 'NONE',  ( 99.99529059433426426, 150.7594456239217777, 1.000000000000006883 ) ) ;
#14387 = DIRECTION ( 'NONE',  ( -0.5000000000000057732, 0.8660254037844353769, 0.000000000000000000 ) ) ;
#14388 = DIRECTION ( 'NONE',  ( -0.000000000000000000, -1.000000000000000000, -0.000000000000000000 ) ) ;
#14389 = LINE ( 'NONE', #20915, #2044 ) ;
#14390 = EDGE_LOOP ( 'NONE', ( #14473, #19295, #19231, #10 ) ) ;
#14391 = FACE_OUTER_BOUND ( 'NONE', #2148, .T. ) ;
#14392 = ORIENTED_EDGE ( 'NONE', *, *, #5014, .T. ) ;
#14393 = VERTEX_POINT ( 'NONE', #5446 ) ;
#14394 = CARTESIAN_POINT ( 'NONE',  ( 210.4088278365934457, 28.82459569483809503, -11.62765399154570289 ) ) ;
#14395 = CARTESIAN_POINT ( 'NONE',  ( 193.6079246875219155, 7.197283639386755638, -8.145074743996337574 ) ) ;
#14396 = FACE_OUTER_BOUND ( 'NONE', #14997, .T. ) ;
#14397 = CARTESIAN_POINT ( 'NONE',  ( -46.99999999999998579, 65.00000000000000000, -22.50000000000000000 ) ) ;
#14398 = FILL_AREA_STYLE ('',( #9274 ) ) ;
#14399 = EDGE_LOOP ( 'NONE', ( #8013, #20288, #13717, #8720 ) ) ;
#14400 = CARTESIAN_POINT ( 'NONE',  ( 198.6701878702990030, 10.11998265067189529, -3.762296834228767484 ) ) ;
#14401 = CARTESIAN_POINT ( 'NONE',  ( 192.0123155716599683, 35.38128320186102371, -18.91295074164679235 ) ) ;
#14402 = CARTESIAN_POINT ( 'NONE',  ( 1.015643852013114135, 51.37805928129599664, -6.209778783225347709 ) ) ;
#14403 = CYLINDRICAL_SURFACE ( 'NONE', #11975, 2.499999999999997780 ) ;
#14404 = DIRECTION ( 'NONE',  ( -0.8660254037844360431, -0.5000000000000044409, 5.976026924694052093E-17 ) ) ;
#14405 = CARTESIAN_POINT ( 'NONE',  ( 30.00000000000000000, 0.000000000000000000, 28.99999999999999645 ) ) ;
#14406 = EDGE_CURVE ( 'NONE', #3434, #6444, #16400, .T. ) ;
#14407 = VECTOR ( 'NONE', #2786, 1000.000000000000000 ) ;
#14408 = ORIENTED_EDGE ( 'NONE', *, *, #19516, .F. ) ;
#14409 = ORIENTED_EDGE ( 'NONE', *, *, #15906, .F. ) ;
#14410 = CARTESIAN_POINT ( 'NONE',  ( 218.5108537097086412, 37.72698357559642801, -16.13347615800331525 ) ) ;
#14411 = PLANE ( 'NONE',  #9497 ) ;
#14412 = CARTESIAN_POINT ( 'NONE',  ( -5.893702928470589519, 79.63451458383713089, -9.058872303765229006 ) ) ;
#14413 = VERTEX_POINT ( 'NONE', #13328 ) ;
#14414 = EDGE_LOOP ( 'NONE', ( #2228, #3463, #4900, #14493, #4736, #18866 ) ) ;
#14415 = ORIENTED_EDGE ( 'NONE', *, *, #2224, .F. ) ;
#14416 = CARTESIAN_POINT ( 'NONE',  ( 105.9489074543212013, 187.9071680446163555, 11.00000000000001066 ) ) ;
#14417 = DIRECTION ( 'NONE',  ( -0.5000000000000054401, 0.8660254037844354880, -0.000000000000000000 ) ) ;
#14418 = CARTESIAN_POINT ( 'NONE',  ( -31.85787517160000704, 63.46251313055055476, 2.426180918394787334 ) ) ;
#14419 = CARTESIAN_POINT ( 'NONE',  ( -28.49950992282111173, 8.571386728324103643, -0.3595220123468740869 ) ) ;
#14420 = VERTEX_POINT ( 'NONE', #8323 ) ;
#14421 = ORIENTED_EDGE ( 'NONE', *, *, #11869, .T. ) ;
#14422 = CARTESIAN_POINT ( 'NONE',  ( 194.6607596192359040, 7.805138170624078775, -8.669480444820575116 ) ) ;
#14423 = VECTOR ( 'NONE', #514, 1000.000000000000114 ) ;
#14425 = EDGE_CURVE ( 'NONE', #6007, #17781, #1773, .T. ) ;
#14424 = CARTESIAN_POINT ( 'NONE',  ( 198.9348002504466137, 6.148758762178306192, -4.550945818102817064 ) ) ;
#14426 = CONICAL_SURFACE ( 'NONE', #2895, 4.171999999999999709, 0.7853981633974687071 ) ;
#14427 = CARTESIAN_POINT ( 'NONE',  ( 220.9239438240024356, 32.06390731203414646, -15.46846178913028425 ) ) ;
#14428 = DIRECTION ( 'NONE',  ( -0.1005394128318207458, -0.05804645706261939847, -0.9932383577419421350 ) ) ;
#14429 = CARTESIAN_POINT ( 'NONE',  ( 0.000000000000000000, 0.000000000000000000, 0.000000000000000000 ) ) ;
#14430 = CARTESIAN_POINT ( 'NONE',  ( 80.75261313425734500, 65.35990508136943333, -25.49604157242841396 ) ) ;
#14431 = EDGE_CURVE ( 'NONE', #1521, #15381, #3770, .T. ) ;
#14432 = CARTESIAN_POINT ( 'NONE',  ( 5.000000000000000000, -2.342598717236899386, 4.057500000000001883 ) ) ;
#14433 = LINE ( 'NONE', #9419, #19101 ) ;
#14434 = DIRECTION ( 'NONE',  ( -0.3886714912512188591, -0.2243995901002276971, 0.8936326403234180482 ) ) ;
#14435 = EDGE_CURVE ( 'NONE', #5032, #15249, #6978, .T. ) ;
#14436 = ORIENTED_EDGE ( 'NONE', *, *, #17248, .F. ) ;
#14437 = B_SPLINE_CURVE_WITH_KNOTS ( 'NONE', 3,
 ( #7466, #15558, #7153, #18511 ),
 .UNSPECIFIED., .F., .F.,
 ( 4, 4 ),
 ( 4.145267925516339689E-07, 0.0005663407490878962338 ),
 .UNSPECIFIED. ) ;
#14438 = AXIS2_PLACEMENT_3D ( 'NONE', #6068, #10738, #17432 ) ;
#14439 = CARTESIAN_POINT ( 'NONE',  ( 78.48791029091835014, 67.03256333895615171, 0.3448344096533276781 ) ) ;
#14440 = ORIENTED_EDGE ( 'NONE', *, *, #7515, .T. ) ;
#14441 = CIRCLE ( 'NONE', #8990, 5.000000000000001776 ) ;
#14442 = ORIENTED_EDGE ( 'NONE', *, *, #3270, .F. ) ;
#14443 = CARTESIAN_POINT ( 'NONE',  ( -0.6518079380778646348, 64.24999999999998579, 2.481238266578627449 ) ) ;
#14444 = B_SPLINE_CURVE_WITH_KNOTS ( 'NONE', 3,
 ( #11786, #20221, #13773, #15482 ),
 .UNSPECIFIED., .F., .F.,
 ( 4, 4 ),
 ( 0.0001001963007107323439, 0.0009541820386879166192 ),
 .UNSPECIFIED. ) ;
#14445 = AXIS2_PLACEMENT_3D ( 'NONE', #1903, #8673, #10135 ) ;
#14446 = DIRECTION ( 'NONE',  ( -0.5000000000000054401, 0.8660254037844354880, -0.000000000000000000 ) ) ;
#14447 = CARTESIAN_POINT ( 'NONE',  ( 222.1003674505514027, 32.15763657739488224, -15.02729838650899907 ) ) ;
#14448 = PRODUCT_CONTEXT ( 'NONE', #14637, 'mechanical' ) ;
#14449 = CARTESIAN_POINT ( 'NONE',  ( 227.0459420597426572, 41.46029532388473626, -17.45257705044830487 ) ) ;
#14450 = ORIENTED_EDGE ( 'NONE', *, *, #2554, .F. ) ;
#14451 = FILL_AREA_STYLE_COLOUR ( '', #13486 ) ;
#14452 = VECTOR ( 'NONE', #4184, 1000.000000000000227 ) ;
#14453 = DIRECTION ( 'NONE',  ( 0.2961981327260293506, 0.1710100716628398243, 0.9396926207859056523 ) ) ;
#14454 = DIRECTION ( 'NONE',  ( -0.8660254037844355990, -0.5000000000000055511, 0.000000000000000000 ) ) ;
#14455 = LINE ( 'NONE', #7856, #3088 ) ;
#14456 = ADVANCED_FACE ( 'NONE', ( #19775 ), #7621, .T. ) ;
#14457 = AXIS2_PLACEMENT_3D ( 'NONE', #10558, #12060, #19786 ) ;
#14458 = ORIENTED_EDGE ( 'NONE', *, *, #8994, .F. ) ;
#14459 = CARTESIAN_POINT ( 'NONE',  ( 226.0372543731067481, 42.55443451360466156, -15.95040389705426875 ) ) ;
#14460 = FACE_OUTER_BOUND ( 'NONE', #5699, .T. ) ;
#14461 = EDGE_CURVE ( 'NONE', #4969, #11211, #6941, .T. ) ;
#14462 = FACE_OUTER_BOUND ( 'NONE', #18182, .T. ) ;
#14463 = DIRECTION ( 'NONE',  ( 0.5000000000000054401, -0.8660254037844354880, 0.000000000000000000 ) ) ;
#14464 = DIRECTION ( 'NONE',  ( 0.8660254037844355990, 0.5000000000000054401, 8.343535232742331521E-16 ) ) ;
#14465 = ORIENTED_EDGE ( 'NONE', *, *, #20447, .T. ) ;
#14466 = B_SPLINE_CURVE_WITH_KNOTS ( 'NONE', 3,
 ( #5910, #14110, #1272, #2962 ),
 .UNSPECIFIED., .F., .F.,
 ( 4, 4 ),
 ( 2.986363092219706325E-07, 0.0004523518780891023312 ),
 .UNSPECIFIED. ) ;
#14467 = PLANE ( 'NONE',  #15601 ) ;
#14468 = CARTESIAN_POINT ( 'NONE',  ( 82.39092640778034138, 58.62218493319811330, -0.5469516794101250134 ) ) ;
#14469 = DIRECTION ( 'NONE',  ( 0.8404609622711977091, 0.000000000000000000, -0.5418720982835085742 ) ) ;
#14470 = CARTESIAN_POINT ( 'NONE',  ( 203.6497874834091704, 1.447950443965099421, -24.35247136794729528 ) ) ;
#14471 = EDGE_CURVE ( 'NONE', #13770, #8261, #5144, .T. ) ;
#14473 = ORIENTED_EDGE ( 'NONE', *, *, #13197, .T. ) ;
#14472 = ORIENTED_EDGE ( 'NONE', *, *, #6963, .F. ) ;
#14474 = EDGE_CURVE ( 'NONE', #18696, #11314, #1685, .T. ) ;
#14475 = AXIS2_PLACEMENT_3D ( 'NONE', #16384, #3139, #6707 ) ;
#14476 = CARTESIAN_POINT ( 'NONE',  ( 214.0936945175409676, 14.36970118611001368, -22.03054070023868860 ) ) ;
#14477 = ORIENTED_EDGE ( 'NONE', *, *, #6571, .F. ) ;
#14478 = DIRECTION ( 'NONE',  ( 0.8660254037844368202, 0.5000000000000032196, 0.000000000000000000 ) ) ;
#14479 = CARTESIAN_POINT ( 'NONE',  ( -28.59745709644790779, 78.78634076744671688, -6.409256716263459275 ) ) ;
#14480 = CARTESIAN_POINT ( 'NONE',  ( 212.2886526734226607, 13.32755979150977943, -4.003039906354141308 ) ) ;
#14481 = EDGE_CURVE ( 'NONE', #19903, #1900, #3558, .T. ) ;
#14482 = ORIENTED_EDGE ( 'NONE', *, *, #17956, .T. ) ;
#14483 = LINE ( 'NONE', #19336, #6827 ) ;
#14484 = ADVANCED_FACE ( 'NONE', ( #18405 ), #9806, .T. ) ;
#14485 = DIRECTION ( 'NONE',  ( -0.8660254037844360431, -0.5000000000000044409, 5.976026924694052093E-17 ) ) ;
#14486 = VECTOR ( 'NONE', #17590, 1000.000000000000114 ) ;
#14487 = CARTESIAN_POINT ( 'NONE',  ( 221.7401889143391713, 32.57550603594015115, -12.00039960601323941 ) ) ;
#14488 = ORIENTED_EDGE ( 'NONE', *, *, #12369, .T. ) ;
#14489 = DIRECTION ( 'NONE',  ( 0.000000000000000000, 0.000000000000000000, -1.000000000000000000 ) ) ;
#14490 = VERTEX_POINT ( 'NONE', #2295 ) ;
#14491 = LINE ( 'NONE', #3228, #12919 ) ;
#14492 = ADVANCED_FACE ( 'NONE', ( #8854 ), #912, .F. ) ;
#14493 = ORIENTED_EDGE ( 'NONE', *, *, #12757, .T. ) ;
#14494 = EDGE_CURVE ( 'NONE', #112, #7973, #8749, .T. ) ;
#14495 = CARTESIAN_POINT ( 'NONE',  ( 209.8252572024504445, 29.79871034852264344, -11.51651525544093602 ) ) ;
#14496 = CARTESIAN_POINT ( 'NONE',  ( 220.3379489458267528, 34.59238660243320851, -17.48830818005197330 ) ) ;
#14497 = FACE_OUTER_BOUND ( 'NONE', #11014, .T. ) ;
#14498 = PLANE ( 'NONE',  #9324 ) ;
#14499 = VECTOR ( 'NONE', #13553, 1000.000000000000227 ) ;
#14500 = CARTESIAN_POINT ( 'NONE',  ( -29.99999999999993605, 5.000000000000018652, -8.526030067124198197 ) ) ;
#14501 = APPLICATION_CONTEXT ( 'automotive_design' ) ;
#14502 = B_SPLINE_CURVE_WITH_KNOTS ( 'NONE', 3,
 ( #432, #11450, #11554, #14762 ),
 .UNSPECIFIED., .F., .F.,
 ( 4, 4 ),
 ( 1.191936099139278000E-06, 0.0005671181583794777459 ),
 .UNSPECIFIED. ) ;
#14503 = ADVANCED_FACE ( 'NONE', ( #5875 ), #19455, .T. ) ;
#14504 = VERTEX_POINT ( 'NONE', #15560 ) ;
#14505 = CIRCLE ( 'NONE', #5655, 4.999999999999997335 ) ;
#14506 = CARTESIAN_POINT ( 'NONE',  ( 212.3836630237427414, 18.03746122203795466, -7.515250618841537111 ) ) ;
#14507 = VERTEX_POINT ( 'NONE', #809 ) ;
#14508 = CARTESIAN_POINT ( 'NONE',  ( 226.3046507595724961, 42.74424951898829761, -15.48400627342726921 ) ) ;
#14509 = CARTESIAN_POINT ( 'NONE',  ( -11.62985761713838606, 45.38383096773601011, -11.71622545425357842 ) ) ;
#14510 = DIRECTION ( 'NONE',  ( 0.8689290541588631234, 0.000000000000000000, 0.4949366614412228360 ) ) ;
#14511 = EDGE_CURVE ( 'NONE', #20444, #19176, #17128, .T. ) ;
#14512 = LINE ( 'NONE', #16399, #16253 ) ;
#14513 = CARTESIAN_POINT ( 'NONE',  ( -25.51376811551812551, 45.02819711329399865, -8.117256888969443196 ) ) ;
#14514 = AXIS2_PLACEMENT_3D ( 'NONE', #17196, #20260, #2784 ) ;
#14516 = ORIENTED_EDGE ( 'NONE', *, *, #3201, .T. ) ;
#14515 = EDGE_LOOP ( 'NONE', ( #9541, #9204, #12175, #11472, #15671 ) ) ;
#14517 = ORIENTED_EDGE ( 'NONE', *, *, #19357, .F. ) ;
#14518 = ORIENTED_EDGE ( 'NONE', *, *, #10430, .T. ) ;
#14519 = CARTESIAN_POINT ( 'NONE',  ( 178.2433706042749009, 57.37193107572242923, -14.00000000000002842 ) ) ;
#14520 = DIRECTION ( 'NONE',  ( -1.000000000000000000, 0.000000000000000000, 0.000000000000000000 ) ) ;
#14521 = AXIS2_PLACEMENT_3D ( 'NONE', #14149, #7755, #14258 ) ;
#14522 = CARTESIAN_POINT ( 'NONE',  ( -5.030706511663012748, 80.00000000026815883, -6.044438231909158077 ) ) ;
#14523 = VERTEX_POINT ( 'NONE', #5767 ) ;
#14524 = VERTEX_POINT ( 'NONE', #15248 ) ;
#14525 = VERTEX_POINT ( 'NONE', #20197 ) ;
#14526 = LINE ( 'NONE', #11322, #1098 ) ;
#14527 = CARTESIAN_POINT ( 'NONE',  ( 0.000000000000000000, -2.342598717236910044, -4.057499999999996554 ) ) ;
#14528 = CARTESIAN_POINT ( 'NONE',  ( 216.1735466947513942, 15.94087575960949010, -13.99568204168108743 ) ) ;
#14529 = CARTESIAN_POINT ( 'NONE',  ( 205.8264633344831225, 9.596613037118636669, -14.00000000000005507 ) ) ;
#14530 = ORIENTED_EDGE ( 'NONE', *, *, #18968, .T. ) ;
#14531 = VERTEX_POINT ( 'NONE', #12046 ) ;
#14532 = LINE ( 'NONE', #9921, #7002 ) ;
#14533 =( NAMED_UNIT ( * ) SI_UNIT ( $, .STERADIAN. ) SOLID_ANGLE_UNIT ( ) );
#14534 = CIRCLE ( 'NONE', #16551, 12.47473710546057823 ) ;
#14535 = CARTESIAN_POINT ( 'NONE',  ( 218.2039718965744441, 38.25851846786385124, -13.17988343266922691 ) ) ;
#14536 = CARTESIAN_POINT ( 'NONE',  ( 30.10683012259193703, 0.000000000000000000, 5.999999999999998224 ) ) ;
#14537 = CARTESIAN_POINT ( 'NONE',  ( -27.65382774999337911, 58.21050512791210707, 4.526042831532911315 ) ) ;
#14538 = CARTESIAN_POINT ( 'NONE',  ( 73.08722033050757716, 69.78136637326532821, -24.59619082723051164 ) ) ;
#14539 = ORIENTED_EDGE ( 'NONE', *, *, #14740, .F. ) ;
#14540 = DIRECTION ( 'NONE',  ( 0.000000000000000000, 0.8532072764867938419, 0.5215719924899993032 ) ) ;
#14541 = DIRECTION ( 'NONE',  ( -0.5000000000000037748, 0.8660254037844364872, 0.000000000000000000 ) ) ;
#14542 = CARTESIAN_POINT ( 'NONE',  ( -29.99999999999999645, -10.00000000000000000, 15.00000000000000000 ) ) ;
#14543 = ORIENTED_EDGE ( 'NONE', *, *, #14071, .T. ) ;
#14544 = CARTESIAN_POINT ( 'NONE',  ( 59.14831028279606073, 75.91136029574231259, -5.422152313826261505 ) ) ;
#14545 = ORIENTED_EDGE ( 'NONE', *, *, #16011, .T. ) ;
#14546 = CIRCLE ( 'NONE', #7749, 5.000000000000002665 ) ;
#14547 = EDGE_LOOP ( 'NONE', ( #14107, #2768, #2432, #4475 ) ) ;
#14548 = CARTESIAN_POINT ( 'NONE',  ( 72.49529059433409373, 198.3908428320658004, 11.00000000000001066 ) ) ;
#14549 = DIRECTION ( 'NONE',  ( -0.3200921998322431850, 0.5544159532159285142, 0.7682212795973754060 ) ) ;
#14550 = PRODUCT_DEFINITION_FORMATION_WITH_SPECIFIED_SOURCE ( 'ANY', '', #15365, .NOT_KNOWN. ) ;
#14551 = ORIENTED_EDGE ( 'NONE', *, *, #11825, .F. ) ;
#14552 = DIRECTION ( 'NONE',  ( -0.8660254037844378194, -0.5000000000000013323, -0.000000000000000000 ) ) ;
#14553 = CARTESIAN_POINT ( 'NONE',  ( 5.000000000000004441, 4.685197434473814759, -6.938893903907228378E-15 ) ) ;
#14554 = VERTEX_POINT ( 'NONE', #5661 ) ;
#14555 = EDGE_CURVE ( 'NONE', #1466, #19163, #18842, .T. ) ;
#14556 = CARTESIAN_POINT ( 'NONE',  ( 5.000000000000000000, -4.506943796211480446E-15, -4.057500000000000107 ) ) ;
#14557 = CARTESIAN_POINT ( 'NONE',  ( 212.7108869958215109, 14.10238615300026410, -22.72623880687309139 ) ) ;
#14558 = CARTESIAN_POINT ( 'NONE',  ( 162.0049095375683237, 13.35563505625637859, -14.00000000000000355 ) ) ;
#14559 = AXIS2_PLACEMENT_3D ( 'NONE', #14400, #19054, #10993 ) ;
#14560 = CARTESIAN_POINT ( 'NONE',  ( 225.8572625086515302, 42.53968280922940437, -16.00491213559311987 ) ) ;
#14561 = DIRECTION ( 'NONE',  ( -0.8660254037844357100, -0.5000000000000051070, 0.000000000000000000 ) ) ;
#14562 = CARTESIAN_POINT ( 'NONE',  ( 182.5734976231970563, 59.87193107572243633, -14.00000000000002842 ) ) ;
#14563 = CARTESIAN_POINT ( 'NONE',  ( 208.4761278624580711, 5.007259451653140125, -14.00000000000005507 ) ) ;
#14564 = CARTESIAN_POINT ( 'NONE',  ( 222.0932163834421829, 32.17002258895639244, -12.92165662794200109 ) ) ;
#14565 = ORIENTED_EDGE ( 'NONE', *, *, #16152, .F. ) ;
#14566 = CARTESIAN_POINT ( 'NONE',  ( 218.3559741392791125, 9.938571268484574617, -21.18305361806777043 ) ) ;
#14567 = AXIS2_PLACEMENT_3D ( 'NONE', #16056, #6368, #2900 ) ;
#14568 = DIRECTION ( 'NONE',  ( 0.6299240516454600591, 0.3636868207865312508, 0.6862416378687270502 ) ) ;
#14569 = ADVANCED_FACE ( 'NONE', ( #2511 ), #7468, .F. ) ;
#14570 = CYLINDRICAL_SURFACE ( 'NONE', #668, 12.47473710546057646 ) ;
#14571 = DIRECTION ( 'NONE',  ( 0.000000000000000000, 6.938893903907178303E-18, 1.000000000000000000 ) ) ;
#14572 = AXIS2_PLACEMENT_3D ( 'NONE', #6542, #3274, #18117 ) ;
#14574 = ORIENTED_EDGE ( 'NONE', *, *, #11072, .F. ) ;
#14573 = EDGE_LOOP ( 'NONE', ( #979, #15702, #19708, #3240 ) ) ;
#14575 = ORIENTED_EDGE ( 'NONE', *, *, #16947, .F. ) ;
#14576 = ORIENTED_EDGE ( 'NONE', *, *, #9786, .F. ) ;
#14577 = ADVANCED_FACE ( 'NONE', ( #7259 ), #2210, .F. ) ;
#14578 = CIRCLE ( 'NONE', #16581, 15.00000000000000000 ) ;
#14579 = CARTESIAN_POINT ( 'NONE',  ( -32.02492996559928429, 68.25592811474751898, 2.150873336511315070 ) ) ;
#14580 = VERTEX_POINT ( 'NONE', #10752 ) ;
#14581 = CARTESIAN_POINT ( 'NONE',  ( 0.000000000000000000, 2.342598717236900718, -4.057500000000001883 ) ) ;
#14582 = ADVANCED_FACE ( 'NONE', ( #12153 ), #7155, .T. ) ;
#14583 = CARTESIAN_POINT ( 'NONE',  ( -27.40890815691616567, 79.34446119967614663, -7.911977669603216690 ) ) ;
#14584 = CARTESIAN_POINT ( 'NONE',  ( 57.15554463217811332, 244.9600622137188850, -13.99999999999998046 ) ) ;
#14585 = FACE_OUTER_BOUND ( 'NONE', #16614, .T. ) ;
#14586 = EDGE_CURVE ( 'NONE', #16809, #15204, #20096, .T. ) ;
#14587 = CARTESIAN_POINT ( 'NONE',  ( 55.44059175264857231, 77.49228655561917378, -16.12265240795897725 ) ) ;
#14588 = CARTESIAN_POINT ( 'NONE',  ( -29.99999999999999645, 5.000000000000000000, -30.00000000000000000 ) ) ;
#14589 = VERTEX_POINT ( 'NONE', #18513 ) ;
#14590 = MECHANICAL_DESIGN_GEOMETRIC_PRESENTATION_REPRESENTATION (  '', ( #4079 ), #11179 ) ;
#14591 = CARTESIAN_POINT ( 'NONE',  ( 49.01452848080091229, 179.0607158131434176, 26.00000000000001776 ) ) ;
#14592 = CARTESIAN_POINT ( 'NONE',  ( 203.8931977501677295, 8.657464312035081377, -1.876704962898965823 ) ) ;
#14593 = AXIS2_PLACEMENT_3D ( 'NONE', #19538, #4914, #1851 ) ;
#14594 = ORIENTED_EDGE ( 'NONE', *, *, #14431, .F. ) ;
#14595 = CARTESIAN_POINT ( 'NONE',  ( 217.6183575532813848, 31.03031750895123864, -14.00000000000004441 ) ) ;
#14596 = EDGE_CURVE ( 'NONE', #11673, #12562, #19839, .T. ) ;
#14597 = CIRCLE ( 'NONE', #18292, 12.47473710546057823 ) ;
#14598 = ORIENTED_EDGE ( 'NONE', *, *, #16034, .F. ) ;
#14599 = CARTESIAN_POINT ( 'NONE',  ( 210.5768882188229725, 28.57253264919412672, -11.75286491306098924 ) ) ;
#14600 = CARTESIAN_POINT ( 'NONE',  ( -15.99999999999999289, 80.00000000000000000, 0.000000000000000000 ) ) ;
#14601 = DIRECTION ( 'NONE',  ( -0.5000000000000051070, 0.8660254037844359321, -0.000000000000000000 ) ) ;
#14602 = CONICAL_SURFACE ( 'NONE', #1375, 4.509097725792825528, 0.5235987755983015912 ) ;
#14603 = EDGE_CURVE ( 'NONE', #9561, #15382, #4302, .T. ) ;
#14604 = CARTESIAN_POINT ( 'NONE',  ( 50.67255043510042611, 99.18893754823274378, -12.49999999999999822 ) ) ;
#14605 = CARTESIAN_POINT ( 'NONE',  ( -28.35376157792325102, 6.482833755044617341, -1.962836280258419164 ) ) ;
#14606 = CIRCLE ( 'NONE', #17979, 11.94520687646042667 ) ;
#14607 = CARTESIAN_POINT ( 'NONE',  ( 227.7069366077078598, 39.98895010731702371, -17.70769053269361137 ) ) ;
#14608 = ORIENTED_EDGE ( 'NONE', *, *, #16615, .T. ) ;
#14609 = AXIS2_PLACEMENT_3D ( 'NONE', #18751, #4224, #12177 ) ;
#14610 = CARTESIAN_POINT ( 'NONE',  ( 68.76802220417130229, 77.60947533363440698, -22.90979173856745277 ) ) ;
#14611 = LINE ( 'NONE', #1555, #4040 ) ;
#14612 = ADVANCED_FACE ( 'NONE', ( #18160 ), #5106, .F. ) ;
#14613 = EDGE_CURVE ( 'NONE', #3756, #13938, #462, .T. ) ;
#14614 = VERTEX_POINT ( 'NONE', #9967 ) ;
#14615 = SURFACE_SIDE_STYLE ('',( #19555 ) ) ;
#14616 = CARTESIAN_POINT ( 'NONE',  ( -11.02792089128730701, 49.53819989913056077, -11.47781853721724232 ) ) ;
#14617 = LINE ( 'NONE', #5996, #17061 ) ;
#14618 = CIRCLE ( 'NONE', #18655, 3.619616396367202782 ) ;
#14619 = CARTESIAN_POINT ( 'NONE',  ( -15.99999999999999289, 15.09941697557068530, 0.9999999999999991118 ) ) ;
#14620 = AXIS2_PLACEMENT_3D ( 'NONE', #5154, #8762, #11845 ) ;
#14621 = DIRECTION ( 'NONE',  ( 0.8660254037844375974, 0.5000000000000019984, -4.996003610813205418E-16 ) ) ;
#14623 = EDGE_LOOP ( 'NONE', ( #18956, #6996, #16190, #15834, #2567, #1802 ) ) ;
#14622 = VERTEX_POINT ( 'NONE', #16461 ) ;
#14624 = EDGE_LOOP ( 'NONE', ( #19947, #4716, #15458, #5448, #13514 ) ) ;
#14625 = PLANE ( 'NONE',  #8137 ) ;
#14626 = DIRECTION ( 'NONE',  ( 0.5000000000000049960, -0.8660254037844358210, 0.000000000000000000 ) ) ;
#14627 = EDGE_CURVE ( 'NONE', #10364, #835, #12375, .T. ) ;
#14628 = CARTESIAN_POINT ( 'NONE',  ( -6.205439792651712416, 80.00000000016144952, -7.778117258980097759 ) ) ;
#14629 = VECTOR ( 'NONE', #2371, 1000.000000000000227 ) ;
#14630 = VERTEX_POINT ( 'NONE', #6803 ) ;
#14631 = ORIENTED_EDGE ( 'NONE', *, *, #20243, .T. ) ;
#14632 = VERTEX_POINT ( 'NONE', #10184 ) ;
#14633 = CARTESIAN_POINT ( 'NONE',  ( 198.5997926933885083, 20.69401370670428619, -1.545471579934808215 ) ) ;
#14634 = CARTESIAN_POINT ( 'NONE',  ( 229.2774278972952118, 37.59524847687330862, -11.12998660979008392 ) ) ;
#14635 = CARTESIAN_POINT ( 'NONE',  ( 209.1514512894397058, 12.04734498975753354, -12.44962402344209274 ) ) ;
#14636 = PLANE ( 'NONE',  #16810 ) ;
#14637 = APPLICATION_CONTEXT ( 'automotive_design' ) ;
#14638 = VERTEX_POINT ( 'NONE', #3945 ) ;
#14639 = VERTEX_POINT ( 'NONE', #13499 ) ;
#14640 = DIRECTION ( 'NONE',  ( 0.5000000000000052180, -0.8660254037844355990, -5.551115123125782086E-17 ) ) ;
#14641 = EDGE_CURVE ( 'NONE', #14622, #14524, #8463, .T. ) ;
#14642 = AXIS2_PLACEMENT_3D ( 'NONE', #11927, #12031, #8732 ) ;
#14643 = DIRECTION ( 'NONE',  ( -0.000000000000000000, -0.000000000000000000, -1.000000000000000000 ) ) ;
#14644 = AXIS2_PLACEMENT_3D ( 'NONE', #11523, #19375, #1675 ) ;
#14645 = AXIS2_PLACEMENT_3D ( 'NONE', #1481, #6026, #4455 ) ;
#14646 = DIRECTION ( 'NONE',  ( -0.5000000000000054401, 0.8660254037844354880, -0.000000000000000000 ) ) ;
#14647 = DIRECTION ( 'NONE',  ( -0.7235536692358585098, -0.4177439057064702421, 0.5495089780708132254 ) ) ;
#14648 = DIRECTION ( 'NONE',  ( 0.5000000000000045519, -0.8660254037844360431, 0.000000000000000000 ) ) ;
#14649 = CIRCLE ( 'NONE', #5462, 15.00000000000001954 ) ;
#14650 = VERTEX_POINT ( 'NONE', #13391 ) ;
#14651 = DIRECTION ( 'NONE',  ( 0.5000000000000046629, -0.8660254037844359321, 0.000000000000000000 ) ) ;
#14652 = FACE_OUTER_BOUND ( 'NONE', #3616, .T. ) ;
#14653 = ORIENTED_EDGE ( 'NONE', *, *, #15838, .T. ) ;
#14654 = EDGE_LOOP ( 'NONE', ( #14834, #20705, #2077, #9703 ) ) ;
#14655 = CARTESIAN_POINT ( 'NONE',  ( 63.92888185421814740, 73.85612640264653805, -2.961109148988000594 ) ) ;
#14656 = VECTOR ( 'NONE', #12764, 1000.000000000000000 ) ;
#14657 = VERTEX_POINT ( 'NONE', #10077 ) ;
#14658 = CARTESIAN_POINT ( 'NONE',  ( -0.1730685457077962841, 65.99841087575602216, 2.475388239833483439 ) ) ;
#14659 = CIRCLE ( 'NONE', #17346, 12.47473710546057823 ) ;
#14660 = AXIS2_PLACEMENT_3D ( 'NONE', #16885, #18476, #16465 ) ;
#14661 = AXIS2_PLACEMENT_3D ( 'NONE', #12487, #20425, #3039 ) ;
#14662 = VERTEX_POINT ( 'NONE', #19630 ) ;
#14663 = CARTESIAN_POINT ( 'NONE',  ( 183.9132435853528307, 37.55142300003367950, -14.00000000000003730 ) ) ;
#14664 = CARTESIAN_POINT ( 'NONE',  ( 34.99529059433364608, 263.3427481158985302, -28.99999999999997513 ) ) ;
#14665 = ORIENTED_EDGE ( 'NONE', *, *, #5085, .T. ) ;
#14666 = FACE_BOUND ( 'NONE', #16842, .T. ) ;
#14667 = DIRECTION ( 'NONE',  ( 0.000000000000000000, 0.000000000000000000, -1.000000000000000000 ) ) ;
#14668 = CARTESIAN_POINT ( 'NONE',  ( 97.00490953756779788, 125.9389375482329569, 55.99999999999997868 ) ) ;
#14669 = ORIENTED_EDGE ( 'NONE', *, *, #186, .F. ) ;
#14670 = CARTESIAN_POINT ( 'NONE',  ( 229.1568300078825473, 37.80413014862199361, -11.35524774226752420 ) ) ;
#14671 = CARTESIAN_POINT ( 'NONE',  ( 208.4761278624580711, 5.007259451653140125, -14.00000000000005507 ) ) ;
#14672 = VECTOR ( 'NONE', #18901, 1000.000000000000227 ) ;
#14673 = DIRECTION ( 'NONE',  ( 0.000000000000000000, 0.000000000000000000, -1.000000000000000000 ) ) ;
#14674 = AXIS2_PLACEMENT_3D ( 'NONE', #6196, #12376, #18835 ) ;
#14675 = CARTESIAN_POINT ( 'NONE',  ( 10.00000000000000178, 9.797174393178825657E-16, -8.000000000000000000 ) ) ;
#14676 = DIRECTION ( 'NONE',  ( -1.000000000000000000, -0.000000000000000000, -0.000000000000000000 ) ) ;
#14677 = ORIENTED_EDGE ( 'NONE', *, *, #2821, .T. ) ;
#14678 = VERTEX_POINT ( 'NONE', #1945 ) ;
#14679 = DIRECTION ( 'NONE',  ( 0.000000000000000000, -0.000000000000000000, 1.000000000000000000 ) ) ;
#14680 = CARTESIAN_POINT ( 'NONE',  ( 64.01501096541383617, 81.30857500227412515, -4.496114496788966797 ) ) ;
#14681 = ADVANCED_FACE ( 'NONE', ( #247 ), #16145, .T. ) ;
#14682 = DIRECTION ( 'NONE',  ( 0.2883401610574364282, -0.4994198088140709424, -0.8169698930104392076 ) ) ;
#14683 = CARTESIAN_POINT ( 'NONE',  ( 75.50233069471819647, 52.62586201590558943, -8.506500717077631890 ) ) ;
#14685 = VERTEX_POINT ( 'NONE', #3525 ) ;
#14684 = ORIENTED_EDGE ( 'NONE', *, *, #18741, .F. ) ;
#14686 = AXIS2_PLACEMENT_3D ( 'NONE', #9280, #6409, #7698 ) ;
#14687 = CARTESIAN_POINT ( 'NONE',  ( -33.31772531566733164, 74.84505238333375132, -1.139833306050677564 ) ) ;
#14688 = VERTEX_POINT ( 'NONE', #20063 ) ;
#14689 = FACE_OUTER_BOUND ( 'NONE', #2806, .T. ) ;
#14690 = CARTESIAN_POINT ( 'NONE',  ( -29.47382129635126802, 77.46132694877815084, -4.041171758127458880 ) ) ;
#14691 = LINE ( 'NONE', #5003, #15412 ) ;
#14692 = ORIENTED_EDGE ( 'NONE', *, *, #5465, .F. ) ;
#14693 = EDGE_CURVE ( 'NONE', #17195, #15282, #17834, .T. ) ;
#14694 = PLANE ( 'NONE',  #81 ) ;
#14695 = CARTESIAN_POINT ( 'NONE',  ( 54.59239912755987945, 77.85276913609830274, -10.53475018185270251 ) ) ;
#14696 = CARTESIAN_POINT ( 'NONE',  ( -28.75894515448919364, 64.25000000000001421, 3.522626389267836000 ) ) ;
#14697 = VERTEX_POINT ( 'NONE', #13290 ) ;
#14698 = AXIS2_PLACEMENT_3D ( 'NONE', #12595, #9490, #4423 ) ;
#14699 = DIRECTION ( 'NONE',  ( 0.000000000000000000, -6.938893903907177533E-18, -1.000000000000000000 ) ) ;
#14700 = EDGE_CURVE ( 'NONE', #13938, #14632, #8393, .T. ) ;
#14701 = CARTESIAN_POINT ( 'NONE',  ( 198.3288405652164670, -0.8512796009538451392, -9.718744748712973447 ) ) ;
#14702 = EDGE_CURVE ( 'NONE', #12799, #16030, #15094, .T. ) ;
#14703 = EDGE_LOOP ( 'NONE', ( #6548, #17581, #4274, #2846 ) ) ;
#14704 = LINE ( 'NONE', #1644, #20017 ) ;
#14705 = ORIENTED_EDGE ( 'NONE', *, *, #20551, .T. ) ;
#14706 = DIRECTION ( 'NONE',  ( 0.5000000000000051070, -0.8660254037844359321, 0.000000000000000000 ) ) ;
#14707 = CARTESIAN_POINT ( 'NONE',  ( 220.6279544895330673, 34.70793063560162750, -17.81526153211079944 ) ) ;
#14708 = PLANE ( 'NONE',  #18860 ) ;
#14709 = DIRECTION ( 'NONE',  ( -0.5000000000000008882, 0.8660254037844381525, 0.000000000000000000 ) ) ;
#14710 = CARTESIAN_POINT ( 'NONE',  ( -26.39516425332331195, 9.975807959609232611, -6.950086042755424742 ) ) ;
#14711 = VECTOR ( 'NONE', #1400, 1000.000000000000000 ) ;
#14712 = VECTOR ( 'NONE', #17394, 1000.000000000000114 ) ;
#14713 = CARTESIAN_POINT ( 'NONE',  ( 226.3611954142891705, 42.31984222815658114, -11.68692323064989047 ) ) ;
#14714 = ORIENTED_EDGE ( 'NONE', *, *, #19505, .T. ) ;
#14715 = CARTESIAN_POINT ( 'NONE',  ( 219.8041001712509512, 35.51703980355691215, -10.43865930680574827 ) ) ;
#14716 = EDGE_CURVE ( 'NONE', #4917, #9963, #3397, .T. ) ;
#14717 = ORIENTED_EDGE ( 'NONE', *, *, #6639, .T. ) ;
#14718 = SURFACE_STYLE_USAGE ( .BOTH. , #14615 ) ;
#14719 = CARTESIAN_POINT ( 'NONE',  ( -3.180065357767781098, 59.84479038527697980, 1.598284787553928776 ) ) ;
#14720 = CARTESIAN_POINT ( 'NONE',  ( -14.13423450066001585, 79.99988027213446173, -12.43461861220364817 ) ) ;
#14721 = EDGE_CURVE ( 'NONE', #11494, #2878, #1841, .T. ) ;
#14722 = DIRECTION ( 'NONE',  ( 0.5000000000000047740, -0.8660254037844359321, 0.000000000000000000 ) ) ;
#14723 = B_SPLINE_CURVE_WITH_KNOTS ( 'NONE', 3,
 ( #13579, #1810, #14765, #6764, #11560, #14868, #9942, #16541, #19707, #18129, #13155, #10047, #18028, #13261 ),
 .UNSPECIFIED., .F., .F.,
 ( 4, 2, 2, 2, 2, 2, 4 ),
 ( 0.000000000000000000, 0.001404861450950249668, 0.002107292176425374503, 0.002809722901900499337, 0.003512153627375624605, 0.004214584352850749005, 0.005619445803801009082 ),
 .UNSPECIFIED. ) ;
#14724 = FACE_OUTER_BOUND ( 'NONE', #705, .T. ) ;
#14726 = ORIENTED_EDGE ( 'NONE', *, *, #15085, .T. ) ;
#14725 = ORIENTED_EDGE ( 'NONE', *, *, #3327, .F. ) ;
#14727 = VERTEX_POINT ( 'NONE', #16777 ) ;
#14728 = ORIENTED_EDGE ( 'NONE', *, *, #18370, .F. ) ;
#14729 = DIRECTION ( 'NONE',  ( -0.8660254037844370423, -0.5000000000000026645, 0.000000000000000000 ) ) ;
#14730 = CARTESIAN_POINT ( 'NONE',  ( 219.4414768585382944, 34.63161541676048927, -10.43865930680574827 ) ) ;
#14731 = EDGE_CURVE ( 'NONE', #4880, #3383, #3837, .T. ) ;
#14732 = EDGE_LOOP ( 'NONE', ( #14653, #9710, #9913, #7081 ) ) ;
#14733 = VERTEX_POINT ( 'NONE', #10288 ) ;
#14734 = LINE ( 'NONE', #9712, #20362 ) ;
#14735 = CARTESIAN_POINT ( 'NONE',  ( 205.4973105777689000, 2.514618399827694972, -26.58724934764007841 ) ) ;
#14736 = EDGE_CURVE ( 'NONE', #9266, #4941, #13032, .T. ) ;
#14737 = CARTESIAN_POINT ( 'NONE',  ( 93.04593889385130012, 210.2557651598135351, 11.00000000000001066 ) ) ;
#14738 = CARTESIAN_POINT ( 'NONE',  ( 218.2182234397639320, 38.46977707783872802, -14.54260449067769301 ) ) ;
#14739 = VERTEX_POINT ( 'NONE', #3625 ) ;
#14740 = EDGE_CURVE ( 'NONE', #12762, #8980, #8713, .T. ) ;
#14741 = ORIENTED_EDGE ( 'NONE', *, *, #16037, .F. ) ;
#14742 = CARTESIAN_POINT ( 'NONE',  ( 220.2180084519553134, 35.41797800104779270, -14.00000000000005507 ) ) ;
#14743 = VECTOR ( 'NONE', #9047, 1000.000000000000000 ) ;
#14744 = FACE_OUTER_BOUND ( 'NONE', #20866, .T. ) ;
#14745 = ADVANCED_FACE ( 'NONE', ( #662 ), #7119, .F. ) ;
#14746 = DIRECTION ( 'NONE',  ( 0.8660254037844369313, 0.5000000000000029976, -4.996003610813203446E-16 ) ) ;
#14747 = CARTESIAN_POINT ( 'NONE',  ( -27.30676186341464273, 66.39265442260771977, 5.329868606387897501 ) ) ;
#14748 = CARTESIAN_POINT ( 'NONE',  ( 220.2180084519553134, 35.41797800104779270, -14.00000000000005507 ) ) ;
#14749 = ORIENTED_EDGE ( 'NONE', *, *, #4769, .T. ) ;
#14750 = LINE ( 'NONE', #3681, #362 ) ;
#14751 = CYLINDRICAL_SURFACE ( 'NONE', #3593, 3.902363844300889451 ) ;
#14752 = VERTEX_POINT ( 'NONE', #9025 ) ;
#14753 = EDGE_CURVE ( 'NONE', #1893, #6192, #15769, .T. ) ;
#14754 = ADVANCED_FACE ( 'NONE', ( #13709 ), #12441, .F. ) ;
#14755 = CARTESIAN_POINT ( 'NONE',  ( 62.39943480050086322, 78.29596884051593975, -12.34141208372355258 ) ) ;
#14756 = ORIENTED_EDGE ( 'NONE', *, *, #18302, .F. ) ;
#14757 = CARTESIAN_POINT ( 'NONE',  ( 210.4416572331711279, 5.884444511168165803, -1.889534153981373921 ) ) ;
#14758 = DIRECTION ( 'NONE',  ( 0.000000000000000000, 0.9557539690135802291, -0.2941672155675891243 ) ) ;
#14759 = EDGE_CURVE ( 'NONE', #5157, #7840, #12222, .T. ) ;
#14760 = TOROIDAL_SURFACE ( 'NONE', #20149, 6.099999999999999645, 0.4000000000000000222 ) ;
#14761 = EDGE_LOOP ( 'NONE', ( #9919, #903, #18196, #281 ) ) ;
#14762 = CARTESIAN_POINT ( 'NONE',  ( 229.7041009120731587, 36.85622913705960002, -14.93232347545832539 ) ) ;
#14763 = ORIENTED_EDGE ( 'NONE', *, *, #4437, .T. ) ;
#14764 = EDGE_CURVE ( 'NONE', #11864, #7993, #11512, .T. ) ;
#14765 = CARTESIAN_POINT ( 'NONE',  ( -27.76006405428915613, 65.74999999999997158, 4.526879896143035431 ) ) ;
#14766 = ORIENTED_EDGE ( 'NONE', *, *, #10815, .T. ) ;
#14767 = DIRECTION ( 'NONE',  ( 0.5000000000000043299, -0.8660254037844361541, 0.000000000000000000 ) ) ;
#14768 = FACE_OUTER_BOUND ( 'NONE', #2154, .T. ) ;
#14769 = ADVANCED_FACE ( 'NONE', ( #18790, #2682, #5840, #9227 ), #4162, .T. ) ;
#14770 = CARTESIAN_POINT ( 'NONE',  ( 216.5584123369822009, 15.79270668264091881, -15.43274561385901045 ) ) ;
#14771 = CARTESIAN_POINT ( 'NONE',  ( 195.0976485947789456, 3.402328959064704783, -12.53629070788332278 ) ) ;
#14772 = AXIS2_PLACEMENT_3D ( 'NONE', #3784, #16728, #15160 ) ;
#14773 = VERTEX_POINT ( 'NONE', #776 ) ;
#14774 = CARTESIAN_POINT ( 'NONE',  ( 5.000000000000004441, 4.685197434473814759, -6.938893903907228378E-15 ) ) ;
#14775 = DIRECTION ( 'NONE',  ( 0.000000000000000000, 6.938893903907177533E-18, 1.000000000000000000 ) ) ;
#14776 = DIRECTION ( 'NONE',  ( 0.8660254037844355990, 0.5000000000000054401, -1.334965637238773043E-14 ) ) ;
#14777 = EDGE_LOOP ( 'NONE', ( #16368, #7914 ) ) ;
#14778 = CONICAL_SURFACE ( 'NONE', #19474, 13.07248899748297433, 0.6693469023067423196 ) ;
#14779 = ADVANCED_FACE ( 'NONE', ( #10614 ), #7226, .T. ) ;
#14780 = CARTESIAN_POINT ( 'NONE',  ( 30.00000000000000000, -10.00000000000000000, 28.99999999999999645 ) ) ;
#14781 = CARTESIAN_POINT ( 'NONE',  ( 82.84955722239773479, 63.45971040577538957, 0.5391910165619532291 ) ) ;
#14782 = DIRECTION ( 'NONE',  ( -0.8660254037844348218, -0.5000000000000064393, 0.000000000000000000 ) ) ;
#14783 = CARTESIAN_POINT ( 'NONE',  ( 78.44171698552800365, 52.99314787609267086, -17.60414262153716791 ) ) ;
#14785 = ORIENTED_EDGE ( 'NONE', *, *, #3841, .T. ) ;
#14784 = ORIENTED_EDGE ( 'NONE', *, *, #16022, .F. ) ;
#14786 = ORIENTED_EDGE ( 'NONE', *, *, #8911, .T. ) ;
#14787 = AXIS2_PLACEMENT_3D ( 'NONE', #1552, #3033, #1449 ) ;
#14788 = VERTEX_POINT ( 'NONE', #981 ) ;
#14789 = AXIS2_PLACEMENT_3D ( 'NONE', #6653, #11447, #5174 ) ;
#14790 = FILL_AREA_STYLE ('',( #5001 ) ) ;
#14791 = TOROIDAL_SURFACE ( 'NONE', #11714, 1.003313105759043200, 1.000000000000000000 ) ;
#14792 = CARTESIAN_POINT ( 'NONE',  ( -31.21251268849638194, 78.92002130297235851, -6.902655774462157723 ) ) ;
#14793 = CARTESIAN_POINT ( 'NONE',  ( 226.6211368133091923, 39.11482588413117867, -14.00000000000005507 ) ) ;
#14794 = DIRECTION ( 'NONE',  ( -0.8660254037844362651, -0.5000000000000043299, 0.000000000000000000 ) ) ;
#14795 = VERTEX_POINT ( 'NONE', #14143 ) ;
#14796 = EDGE_CURVE ( 'NONE', #7744, #3819, #6588, .T. ) ;
#14797 = DIRECTION ( 'NONE',  ( 0.000000000000000000, -0.000000000000000000, 1.000000000000000000 ) ) ;
#14798 = CARTESIAN_POINT ( 'NONE',  ( 80.18983717961930324, 65.86547942624545726, 0.4720184283333879183 ) ) ;
#14799 = CARTESIAN_POINT ( 'NONE',  ( 57.15554463217811332, 244.9600622137188850, -13.99999999999998046 ) ) ;
#14800 = VERTEX_POINT ( 'NONE', #20470 ) ;
#14801 = AXIS2_PLACEMENT_3D ( 'NONE', #4904, #11376, #16254 ) ;
#14802 = CARTESIAN_POINT ( 'NONE',  ( 221.2452766128280075, 31.50734259565048845, -15.69686519029809446 ) ) ;
#14803 = CIRCLE ( 'NONE', #11391, 11.94520687646042667 ) ;
#14804 = ORIENTED_EDGE ( 'NONE', *, *, #1207, .T. ) ;
#14805 = CARTESIAN_POINT ( 'NONE',  ( 227.9553588074475670, 39.88513931160575510, -14.00000000000005507 ) ) ;
#14806 = ADVANCED_FACE ( 'NONE', ( #1193 ), #20577, .F. ) ;
#14808 = ORIENTED_EDGE ( 'NONE', *, *, #11959, .T. ) ;
#14807 = ORIENTED_EDGE ( 'NONE', *, *, #10976, .T. ) ;
#14809 = LINE ( 'NONE', #258, #17362 ) ;
#14810 = CARTESIAN_POINT ( 'NONE',  ( 219.9824452441442304, 35.62000737940047657, -10.21862775258421152 ) ) ;
#14811 = LINE ( 'NONE', #1651, #1924 ) ;
#14812 =( BOUNDED_SURFACE ( )  B_SPLINE_SURFACE ( 3, 2, ( 
 ( #7998, #6504, #8093 ),
 ( #16386, #11299, #19762 ),
 ( #14710, #8413, #19443 ),
 ( #14913, #1861, #8307 ),
 ( #17769, #6400, #14500 ),
 ( #3141, #20927, #9587 ),
 ( #19653, #6709, #3236 ),
 ( #16085, #5129, #11614 ),
 ( #18078, #69, #1553 ),
 ( #9691, #16482, #12898 ),
 ( #1964, #1653, #13314 ),
 ( #4925, #14605, #11194 ),
 ( #11400, #15342, #17015 ),
 ( #2496, #4072, #7248 ),
 ( #15234, #16587, #3969 ),
 ( #19861, #796, #10097 ),
 ( #18499, #11717, #10419 ),
 ( #15441, #2383, #20185 ),
 ( #18280, #13732, #5227 ),
 ( #900, #12036, #5647 ),
 ( #7141, #5328, #18180 ),
 ( #12137, #8529, #3752 ),
 ( #2280, #11819, #15028 ),
 ( #20083, #487, #6927 ),
 ( #10208, #2180, #16701 ),
 ( #8632, #15130, #585 ),
 ( #11933, #19966, #5432 ),
 ( #18393, #3862, #10311 ) ),
 .UNSPECIFIED., .F., .F., .F. ) 
 B_SPLINE_SURFACE_WITH_KNOTS ( ( 4, 2, 2, 2, 2, 2, 2, 2, 2, 2, 2, 2, 2, 4 ),
 ( 3, 3 ),
 ( 0.009371192738994881324, 0.01079808352755677603, 0.01222497431611867247, 0.01365186510468056891, 0.01507875589324246535, 0.01793253747036625823, 0.01935942825892815466, 0.02078631904749004763, 0.02221320983605194060, 0.02364010062461383704, 0.02649388220173762992, 0.02934766377886142280, 0.03077455456742331924, 0.03220144535598521568 ),
 ( 0.000000000000000000, 1.000000000000000000 ),
 .UNSPECIFIED. ) 
 GEOMETRIC_REPRESENTATION_ITEM ( )  RATIONAL_B_SPLINE_SURFACE ( (
 ( 1.000000000000000000, 0.7071067811865479058, 1.000000000000000000),
 ( 1.000000000000000000, 0.7232527279161264921, 1.000000000000000000),
 ( 1.000000000000000000, 0.7388286583289560561, 1.000000000000000000),
 ( 1.000000000000000000, 0.7685446699867291009, 1.000000000000000000),
 ( 1.000000000000000000, 0.7826850257046925607, 1.000000000000000000),
 ( 1.000000000000000000, 0.8093023715178216948, 1.000000000000000000),
 ( 1.000000000000000000, 0.8217945561033374036, 1.000000000000000000),
 ( 1.000000000000000000, 0.8445755018420567639, 1.000000000000000000),
 ( 1.000000000000000000, 0.8549247766998627762, 1.000000000000000000),
 ( 1.000000000000000000, 0.8828010807230063373, 1.000000000000000000),
 ( 1.000000000000000000, 0.8971838639936082771, 1.000000000000000000),
 ( 1.000000000000000000, 0.9119221572953989385, 1.000000000000000000),
 ( 1.000000000000000000, 0.9157004699627206978, 1.000000000000000000),
 ( 1.000000000000000000, 0.9207044786150797577, 1.000000000000000000),
 ( 1.000000000000000000, 0.9219484747058886986, 1.000000000000000000),
 ( 1.000000000000000000, 0.9219603739042575574, 1.000000000000000000),
 ( 1.000000000000000000, 0.9207283435489677093, 1.000000000000000000),
 ( 1.000000000000000000, 0.9158001944594933441, 1.000000000000000000),
 ( 1.000000000000000000, 0.9120921721005434968, 1.000000000000000000),
 ( 1.000000000000000000, 0.8973220332527075405, 1.000000000000000000),
 ( 1.000000000000000000, 0.8828883913922480620, 1.000000000000000000),
 ( 1.000000000000000000, 0.8457423740019180958, 1.000000000000000000),
 ( 1.000000000000000000, 0.8230077850553781937, 1.000000000000000000),
 ( 1.000000000000000000, 0.7829299428437686004, 1.000000000000000000),
 ( 1.000000000000000000, 0.7686927448236463567, 1.000000000000000000),
 ( 1.000000000000000000, 0.7388689099750124223, 1.000000000000000000),
 ( 1.000000000000000000, 0.7232573842950190679, 1.000000000000000000),
 ( 1.000000000000000000, 0.7071067811865474617, 1.000000000000000000) ) ) 
 REPRESENTATION_ITEM ( '' )  SURFACE ( )  );
#14813 = DIRECTION ( 'NONE',  ( -0.000000000000000000, -1.000000000000000000, -0.000000000000000000 ) ) ;
#14814 = LINE ( 'NONE', #164, #9387 ) ;
#14815 = CARTESIAN_POINT ( 'NONE',  ( 221.3433106695783295, 31.33754262848677996, -15.14518239232902985 ) ) ;
#14816 = ORIENTED_EDGE ( 'NONE', *, *, #8777, .F. ) ;
#14817 = VECTOR ( 'NONE', #16225, 1000.000000000000114 ) ;
#14818 = EDGE_CURVE ( 'NONE', #5234, #1744, #7540, .T. ) ;
#14819 = CARTESIAN_POINT ( 'NONE',  ( 79.37802773247075550, 66.47170366897312022, -25.42092142087688700 ) ) ;
#14820 = DIRECTION ( 'NONE',  ( 0.5000000000000054401, -0.8660254037844354880, 0.000000000000000000 ) ) ;
#14821 = ORIENTED_EDGE ( 'NONE', *, *, #5970, .T. ) ;
#14822 = CARTESIAN_POINT ( 'NONE',  ( 226.1187385850312523, 42.73978977507332644, -15.51567023025815395 ) ) ;
#14823 = CARTESIAN_POINT ( 'NONE',  ( -3.812720765152911806, 52.63858550657156599, -3.991166449876146327 ) ) ;
#14824 = CARTESIAN_POINT ( 'NONE',  ( -12.28221561448063781, 79.99809398375025182, -12.23915253492440947 ) ) ;
#14825 = LINE ( 'NONE', #6410, #2376 ) ;
#14826 = DIRECTION ( 'NONE',  ( -0.5000000000000054401, 0.8660254037844354880, -0.000000000000000000 ) ) ;
#14828 = ORIENTED_EDGE ( 'NONE', *, *, #20614, .F. ) ;
#14827 = ORIENTED_EDGE ( 'NONE', *, *, #9378, .T. ) ;
#14829 = VERTEX_POINT ( 'NONE', #17304 ) ;
#14830 = ORIENTED_EDGE ( 'NONE', *, *, #18247, .F. ) ;
#14831 = CARTESIAN_POINT ( 'NONE',  ( 201.2754665570134591, 0.5923418568450431465, -22.94176278698363092 ) ) ;
#14832 = DIRECTION ( 'NONE',  ( -0.8660254037844380415, -0.5000000000000014433, -0.000000000000000000 ) ) ;
#14833 = EDGE_CURVE ( 'NONE', #2143, #9868, #18578, .T. ) ;
#14834 = ORIENTED_EDGE ( 'NONE', *, *, #14753, .T. ) ;
#14835 = ORIENTED_EDGE ( 'NONE', *, *, #18211, .T. ) ;
#14836 = CONICAL_SURFACE ( 'NONE', #5651, 13.07248899748297433, 0.6693469023067423196 ) ;
#14837 = CARTESIAN_POINT ( 'NONE',  ( 76.19073749086850000, 131.9901410505959518, 41.00000000000001421 ) ) ;
#14838 = PLANE ( 'NONE',  #14960 ) ;
#14839 = CARTESIAN_POINT ( 'NONE',  ( 208.4761278624580711, 5.007259451653140125, -14.00000000000005507 ) ) ;
#14840 = CARTESIAN_POINT ( 'NONE',  ( 218.2525276197119126, 38.61631259782608083, -14.55011169161688933 ) ) ;
#14841 = ORIENTED_EDGE ( 'NONE', *, *, #18769, .F. ) ;
#14842 = ORIENTED_EDGE ( 'NONE', *, *, #1626, .F. ) ;
#14843 = DIRECTION ( 'NONE',  ( -0.5943026915289566503, -0.3431208189343674109, 0.7273736415730548410 ) ) ;
#14844 = EDGE_CURVE ( 'NONE', #13380, #13321, #4587, .T. ) ;
#14845 = ORIENTED_EDGE ( 'NONE', *, *, #18186, .F. ) ;
#14846 = ADVANCED_FACE ( 'NONE', ( #7426 ), #10500, .F. ) ;
#14847 = B_SPLINE_CURVE_WITH_KNOTS ( 'NONE', 3,
 ( #2125, #20333, #6977, #13464 ),
 .UNSPECIFIED., .F., .F.,
 ( 4, 4 ),
 ( 1.122767056962631348E-06, 0.0008551085050396736416 ),
 .UNSPECIFIED. ) ;
#14848 = CYLINDRICAL_SURFACE ( 'NONE', #16564, 12.47473710546057646 ) ;
#14849 = VECTOR ( 'NONE', #7792, 1000.000000000000000 ) ;
#14850 = CARTESIAN_POINT ( 'NONE',  ( 208.2336538649943236, 4.094446933302576142, -25.81526893633797570 ) ) ;
#14851 = CARTESIAN_POINT ( 'NONE',  ( -27.62855338901809787, 51.88754995109739099, -5.120729935976574332 ) ) ;
#14852 = CARTESIAN_POINT ( 'NONE',  ( -19.30416908549006649, 18.86621361051762591, 12.05778820527624262 ) ) ;
#14853 = AXIS2_PLACEMENT_3D ( 'NONE', #1102, #17417, #17628 ) ;
#14854 = LINE ( 'NONE', #16215, #12781 ) ;
#14855 = DIRECTION ( 'NONE',  ( -0.8660254037844360431, -0.5000000000000044409, -4.336808689942049290E-16 ) ) ;
#14856 = ADVANCED_FACE ( 'NONE', ( #875, #7325 ), #13814, .T. ) ;
#14857 = ORIENTED_EDGE ( 'NONE', *, *, #19751, .T. ) ;
#14858 = CARTESIAN_POINT ( 'NONE',  ( 69.07465262935465944, 74.30594400923098419, -3.091493055308389248 ) ) ;
#14859 = ORIENTED_EDGE ( 'NONE', *, *, #17572, .T. ) ;
#14860 = DIRECTION ( 'NONE',  ( -0.5000000000000054401, 0.8660254037844354880, -0.000000000000000000 ) ) ;
#14861 = DIRECTION ( 'NONE',  ( 0.000000000000000000, -0.5000000000000013323, -0.8660254037844378194 ) ) ;
#14862 = EDGE_CURVE ( 'NONE', #18411, #9311, #7272, .T. ) ;
#14863 = CIRCLE ( 'NONE', #9064, 5.999999999999998224 ) ;
#14864 = ORIENTED_EDGE ( 'NONE', *, *, #12555, .T. ) ;
#14865 = CARTESIAN_POINT ( 'NONE',  ( 205.5718816476997688, 14.10467741091863658, -2.341985411377013548 ) ) ;
#14866 = EDGE_CURVE ( 'NONE', #8535, #11414, #10327, .T. ) ;
#14867 =( GEOMETRIC_REPRESENTATION_CONTEXT ( 3 ) GLOBAL_UNCERTAINTY_ASSIGNED_CONTEXT ( ( #13179 ) ) GLOBAL_UNIT_ASSIGNED_CONTEXT ( ( #4291, #20605, #19034 ) ) REPRESENTATION_CONTEXT ( 'NONE', 'WORKASPACE' ) );
#14868 = CARTESIAN_POINT ( 'NONE',  ( -28.75604140624042770, 65.74999999999997158, 3.524958307384044698 ) ) ;
#14869 = ORIENTED_EDGE ( 'NONE', *, *, #8959, .T. ) ;
#14870 = CARTESIAN_POINT ( 'NONE',  ( 85.60317707801368670, 145.6873174624877834, 41.00000000000001421 ) ) ;
#14871 = DIRECTION ( 'NONE',  ( 0.7500000000000015543, 0.4330127018922264037, 0.4999999999999917288 ) ) ;
#14872 = CARTESIAN_POINT ( 'NONE',  ( 222.0250846156424984, 32.08205220642481237, -13.96598824437089803 ) ) ;
#14873 = CARTESIAN_POINT ( 'NONE',  ( 195.0230240956219347, 3.359244484388281826, -14.00000000000005507 ) ) ;
#14874 = EDGE_CURVE ( 'NONE', #1492, #15273, #20783, .T. ) ;
#14875 = ORIENTED_EDGE ( 'NONE', *, *, #12429, .F. ) ;
#14876 = DIRECTION ( 'NONE',  ( -0.8660254037844370423, -0.5000000000000027756, -1.818545872641207967E-15 ) ) ;
#14877 = CARTESIAN_POINT ( 'NONE',  ( 208.0983737146324870, 5.661548828456886895, -14.00000000000005507 ) ) ;
#14878 = DIRECTION ( 'NONE',  ( -0.5000000000000054401, 0.8660254037844354880, -0.000000000000000000 ) ) ;
#14879 = ADVANCED_FACE ( 'NONE', ( #16229 ), #20880, .T. ) ;
#14880 = ORIENTED_EDGE ( 'NONE', *, *, #11042, .T. ) ;
#14881 = DIRECTION ( 'NONE',  ( -0.8660254037844360431, -0.5000000000000044409, 5.976026924694052093E-17 ) ) ;
#14882 = EDGE_CURVE ( 'NONE', #16846, #16240, #17592, .T. ) ;
#14883 = CARTESIAN_POINT ( 'NONE',  ( 199.2144802262915846, 21.04890371929339921, -14.00000000000005507 ) ) ;
#14884 = CARTESIAN_POINT ( 'NONE',  ( 20.67255043510014900, 151.1504617752989361, -12.49999999999999822 ) ) ;
#14885 = CARTESIAN_POINT ( 'NONE',  ( 79.59702692428714954, 50.14740214866447587, -16.24970959789619940 ) ) ;
#14886 = EDGE_CURVE ( 'NONE', #15521, #11736, #10994, .T. ) ;
#14888 = ORIENTED_EDGE ( 'NONE', *, *, #11068, .F. ) ;
#14887 = ORIENTED_EDGE ( 'NONE', *, *, #5843, .T. ) ;
#14889 = VERTEX_POINT ( 'NONE', #12742 ) ;
#14890 = CARTESIAN_POINT ( 'NONE',  ( 34.99529059433364608, 263.3427481158985302, -28.99999999999997513 ) ) ;
#14891 = VECTOR ( 'NONE', #322, 1000.000000000000000 ) ;
#14892 = VERTEX_POINT ( 'NONE', #11044 ) ;
#14893 = CARTESIAN_POINT ( 'NONE',  ( 76.11375628839972762, 53.44186132163859071, -6.514818636118950401 ) ) ;
#14894 = EDGE_CURVE ( 'NONE', #11548, #8298, #3230, .T. ) ;
#14895 = CARTESIAN_POINT ( 'NONE',  ( -26.76057640522419590, 79.79422864173648122, -10.01493943371489159 ) ) ;
#14896 = CARTESIAN_POINT ( 'NONE',  ( 202.1791022559531541, 13.45620526910692938, -29.00000000000009237 ) ) ;
#14897 = DIRECTION ( 'NONE',  ( 0.8660254037844373753, 0.5000000000000022204, 0.000000000000000000 ) ) ;
#14898 = ORIENTED_EDGE ( 'NONE', *, *, #15660, .F. ) ;
#14899 = DIRECTION ( 'NONE',  ( 0.5000000000000054401, -0.8660254037844354880, 0.000000000000000000 ) ) ;
#14900 = CARTESIAN_POINT ( 'NONE',  ( 64.97908659311265467, 73.40006927592642683, -2.567007515994158773 ) ) ;
#14901 = DIRECTION ( 'NONE',  ( 1.000000000000000000, 0.000000000000000000, 0.000000000000000000 ) ) ;
#14902 = ORIENTED_EDGE ( 'NONE', *, *, #8590, .T. ) ;
#14903 = FACE_OUTER_BOUND ( 'NONE', #1369, .T. ) ;
#14904 = DIRECTION ( 'NONE',  ( 0.8660254037844361541, 0.5000000000000044409, 0.000000000000000000 ) ) ;
#14905 = CIRCLE ( 'NONE', #17931, 3.902363844300875240 ) ;
#14906 = DIRECTION ( 'NONE',  ( -0.5000000000000047740, 0.8660254037844358210, 0.000000000000000000 ) ) ;
#14907 = ORIENTED_EDGE ( 'NONE', *, *, #17876, .F. ) ;
#14908 = LINE ( 'NONE', #8836, #11558 ) ;
#14909 = CARTESIAN_POINT ( 'NONE',  ( 212.0555786093015911, 13.72404367964075789, -3.627669900420236626 ) ) ;
#14910 = CARTESIAN_POINT ( 'NONE',  ( -32.77319314005540463, 77.96684442108207236, -4.956410556015048208 ) ) ;
#14911 = VECTOR ( 'NONE', #12863, 1000.000000000000000 ) ;
#14912 = CARTESIAN_POINT ( 'NONE',  ( 72.22890356904881060, 74.87903105603933795, -24.07778875527023743 ) ) ;
#14913 = CARTESIAN_POINT ( 'NONE',  ( -26.75388419629425130, 9.893953324963231211, -6.380996046697354096 ) ) ;
#14914 = CARTESIAN_POINT ( 'NONE',  ( 198.8341126585713425, -1.332380712484759755, -16.70797078425209747 ) ) ;
#14915 = VERTEX_POINT ( 'NONE', #14557 ) ;
#14916 = CARTESIAN_POINT ( 'NONE',  ( 77.89229590160842065, 55.87094247655682011, -21.76811895496497584 ) ) ;
#14917 = VECTOR ( 'NONE', #19117, 1000.000000000000114 ) ;
#14918 = CARTESIAN_POINT ( 'NONE',  ( 219.2715103217157662, 36.85138278592162209, -10.61701699970689639 ) ) ;
#14919 = VECTOR ( 'NONE', #12367, 1000.000000000000000 ) ;
#14920 = VERTEX_POINT ( 'NONE', #19208 ) ;
#14921 = CARTESIAN_POINT ( 'NONE',  ( 203.3234976231972553, 23.93187681866832861, -14.00000000000004441 ) ) ;
#14922 = CARTESIAN_POINT ( 'NONE',  ( -3.058993387607990666, 55.97632480169432512, -0.5003277293098231659 ) ) ;
#14923 = CARTESIAN_POINT ( 'NONE',  ( -1.033406382133238655, 79.01409684087832375, -7.140683506250414148 ) ) ;
#14924 = DIRECTION ( 'NONE',  ( 0.5000000000000054401, -0.8660254037844354880, 0.000000000000000000 ) ) ;
#14925 = CARTESIAN_POINT ( 'NONE',  ( 208.2480327748888556, 26.26442771496472162, -20.84195174293596153 ) ) ;
#14926 = LINE ( 'NONE', #5342, #177 ) ;
#14928 = ORIENTED_EDGE ( 'NONE', *, *, #10826, .T. ) ;
#14927 = EDGE_LOOP ( 'NONE', ( #10925, #16837, #17686, #6105, #12159 ) ) ;
#14929 = EDGE_LOOP ( 'NONE', ( #1617, #16897, #7580, #3903 ) ) ;
#14930 = ORIENTED_EDGE ( 'NONE', *, *, #6956, .F. ) ;
#14931 = CARTESIAN_POINT ( 'NONE',  ( -15.99999999999999289, 10.09941697557069418, 4.999999999999989342 ) ) ;
#14932 = AXIS2_PLACEMENT_3D ( 'NONE', #420, #16326, #6865 ) ;
#14933 = DIRECTION ( 'NONE',  ( 0.000000000000000000, -0.4999999999999985567, 0.8660254037844393737 ) ) ;
#14934 = VECTOR ( 'NONE', #4891, 1000.000000000000000 ) ;
#14935 = ORIENTED_EDGE ( 'NONE', *, *, #2443, .F. ) ;
#14936 = VERTEX_POINT ( 'NONE', #12647 ) ;
#14937 = EDGE_CURVE ( 'NONE', #19670, #1594, #20, .T. ) ;
#14938 = DIRECTION ( 'NONE',  ( -0.8660254037844359321, -0.5000000000000045519, 5.976026924694053325E-17 ) ) ;
#14939 = CARTESIAN_POINT ( 'NONE',  ( 61.99529059433385925, 216.5773763115390125, -5.999999999999973355 ) ) ;
#14940 = VECTOR ( 'NONE', #20048, 1000.000000000000114 ) ;
#14941 = CARTESIAN_POINT ( 'NONE',  ( 214.8856909933734300, 7.826610718103062858, -14.00000000000005507 ) ) ;
#14942 = VERTEX_POINT ( 'NONE', #19501 ) ;
#14943 = AXIS2_PLACEMENT_3D ( 'NONE', #14519, #3047, #17577 ) ;
#14944 = CARTESIAN_POINT ( 'NONE',  ( 215.3464568589922408, 15.62403312296995317, -9.340893379680396791 ) ) ;
#14945 = PLANE ( 'NONE',  #10384 ) ;
#14946 = ORIENTED_EDGE ( 'NONE', *, *, #5390, .F. ) ;
#14947 = VECTOR ( 'NONE', #1265, 1000.000000000000000 ) ;
#14948 = ORIENTED_EDGE ( 'NONE', *, *, #7277, .T. ) ;
#14949 = DIRECTION ( 'NONE',  ( 0.5000000000000044409, -0.8660254037844360431, 0.000000000000000000 ) ) ;
#14950 = TOROIDAL_SURFACE ( 'NONE', #13241, 6.960520131757804485, 1.000000000000000000 ) ;
#14951 = LINE ( 'NONE', #3271, #17671 ) ;
#14952 = CARTESIAN_POINT ( 'NONE',  ( -33.46931044135702393, 53.99090883974105282, -2.305310864414939598 ) ) ;
#14953 = CARTESIAN_POINT ( 'NONE',  ( 41.50490953756720813, 222.0677573683055925, -19.00000000000000355 ) ) ;
#14954 = CIRCLE ( 'NONE', #4775, 12.47473710546057823 ) ;
#14955 = FACE_OUTER_BOUND ( 'NONE', #453, .T. ) ;
#14956 = VECTOR ( 'NONE', #15119, 1000.000000000000000 ) ;
#14957 = CARTESIAN_POINT ( 'NONE',  ( 198.6079246875219724, -1.462970398457601240, -8.145074743996339350 ) ) ;
#14958 = ORIENTED_EDGE ( 'NONE', *, *, #3416, .F. ) ;
#14959 = CARTESIAN_POINT ( 'NONE',  ( 59.12621987370580001, 85.07716061577534106, -9.825189264790521904 ) ) ;
#14960 = AXIS2_PLACEMENT_3D ( 'NONE', #3260, #19570, #6630 ) ;
#14961 = EDGE_CURVE ( 'NONE', #456, #11494, #19107, .T. ) ;
#14962 = ORIENTED_EDGE ( 'NONE', *, *, #9775, .F. ) ;
#14963 = ORIENTED_EDGE ( 'NONE', *, *, #5654, .F. ) ;
#14964 = ADVANCED_FACE ( 'NONE', ( #9434 ), #17450, .T. ) ;
#14965 = ORIENTED_EDGE ( 'NONE', *, *, #5437, .F. ) ;
#14966 = LINE ( 'NONE', #19804, #7800 ) ;
#14967 = DIRECTION ( 'NONE',  ( 0.8660254037844359321, 0.5000000000000046629, 0.000000000000000000 ) ) ;
#14968 = AXIS2_PLACEMENT_3D ( 'NONE', #6298, #11296, #9583 ) ;
#14969 = VERTEX_POINT ( 'NONE', #323 ) ;
#14970 = CARTESIAN_POINT ( 'NONE',  ( 220.2282753091644167, 34.75232210732326621, -17.51488284254729066 ) ) ;
#14971 = ORIENTED_EDGE ( 'NONE', *, *, #833, .T. ) ;
#14972 = CONTEXT_DEPENDENT_SHAPE_REPRESENTATION ( #5387, #4168 ) ;
#14973 = AXIS2_PLACEMENT_3D ( 'NONE', #14416, #1469, #20845 ) ;
#14974 = DIRECTION ( 'NONE',  ( 0.8660254037844358210, 0.5000000000000047740, 0.000000000000000000 ) ) ;
#14975 = EDGE_CURVE ( 'NONE', #18631, #14630, #19814, .T. ) ;
#14976 = VERTEX_POINT ( 'NONE', #19921 ) ;
#14977 = CARTESIAN_POINT ( 'NONE',  ( 212.8906072256780533, 14.02913777190325817, -22.83852658738941699 ) ) ;
#14978 = LINE ( 'NONE', #16650, #11020 ) ;
#14979 = VERTEX_POINT ( 'NONE', #11775 ) ;
#14980 = LINE ( 'NONE', #13369, #16115 ) ;
#14981 = CARTESIAN_POINT ( 'NONE',  ( 207.5029616403657258, 10.91857914292485532, -25.96288910428604879 ) ) ;
#14982 = ADVANCED_FACE ( 'NONE', ( #14768 ), #13582, .F. ) ;
#14983 = ORIENTED_EDGE ( 'NONE', *, *, #17981, .F. ) ;
#14984 = DIRECTION ( 'NONE',  ( 0.5000000000000051070, -0.8660254037844359321, 0.000000000000000000 ) ) ;
#14985 = PRESENTATION_LAYER_ASSIGNMENT (  '', '', ( #7839 ) ) ;
#14986 = DIRECTION ( 'NONE',  ( 0.000000000000000000, 0.000000000000000000, 1.000000000000000000 ) ) ;
#14987 = CARTESIAN_POINT ( 'NONE',  ( 62.36389338619030553, 105.9389375482328006, 4.000000000000000000 ) ) ;
#14988 = EDGE_LOOP ( 'NONE', ( #1988, #16562, #16694, #11848 ) ) ;
#14989 = VECTOR ( 'NONE', #10081, 1000.000000000000000 ) ;
#14990 = LINE ( 'NONE', #16553, #1724 ) ;
#14991 = ADVANCED_FACE ( 'NONE', ( #15188 ), #14760, .T. ) ;
#14992 = CARTESIAN_POINT ( 'NONE',  ( 190.8575367324608010, 36.14736977200433898, -9.000000000000063949 ) ) ;
#14993 = VECTOR ( 'NONE', #14746, 1000.000000000000114 ) ;
#14994 = CARTESIAN_POINT ( 'NONE',  ( -12.79128543553366093, 69.99684855425128660, -3.836613224171032233 ) ) ;
#14995 = CARTESIAN_POINT ( 'NONE',  ( 78.02789439511529679, 52.20891951634391859, -14.88908151311502870 ) ) ;
#14996 = ORIENTED_EDGE ( 'NONE', *, *, #5108, .F. ) ;
#14997 = EDGE_LOOP ( 'NONE', ( #14440, #11580, #1109, #19986 ) ) ;
#14998 = EDGE_CURVE ( 'NONE', #16413, #13880, #10264, .T. ) ;
#14999 = LINE ( 'NONE', #352, #9341 ) ;
#15000 = EDGE_CURVE ( 'NONE', #5382, #1746, #8971, .T. ) ;
#15001 = ORIENTED_EDGE ( 'NONE', *, *, #19568, .F. ) ;
#15002 = CARTESIAN_POINT ( 'NONE',  ( 77.63095968975100902, 55.50711545842607819, -21.40358471902519000 ) ) ;
#15003 = CIRCLE ( 'NONE', #428, 3.619616396367202782 ) ;
#15004 = CARTESIAN_POINT ( 'NONE',  ( -19.59011831531341841, 79.99589872796802581, -12.11680902303608853 ) ) ;
#15005 = CARTESIAN_POINT ( 'NONE',  ( 198.4225180578738161, 5.321943238602927728, -4.915515517929134326 ) ) ;
#15006 = LINE ( 'NONE', #7120, #2713 ) ;
#15007 = EDGE_LOOP ( 'NONE', ( #16547, #13623, #16950, #6900, #9608 ) ) ;
#15008 = AXIS2_PLACEMENT_3D ( 'NONE', #5643, #19962, #7136 ) ;
#15009 = DIRECTION ( 'NONE',  ( 0.5000000000000046629, -0.8660254037844359321, -6.938893903907214573E-16 ) ) ;
#15010 = ADVANCED_FACE ( 'NONE', ( #16342 ), #2911, .T. ) ;
#15011 = CARTESIAN_POINT ( 'NONE',  ( 55.76083050669604546, 77.35608213855016402, -8.438634470110439878 ) ) ;
#15012 = LINE ( 'NONE', #10084, #19868 ) ;
#15013 = PRODUCT_DEFINITION_SHAPE ( 'NONE', 'NONE',  #15369 ) ;
#15014 = ORIENTED_EDGE ( 'NONE', *, *, #324, .T. ) ;
#15015 = CARTESIAN_POINT ( 'NONE',  ( 218.9002013747199555, 37.08263844404898180, -11.10922658182122902 ) ) ;
#15016 = CARTESIAN_POINT ( 'NONE',  ( 192.4890135470689074, 6.551279991246921064, -15.47241223419981537 ) ) ;
#15017 = DIRECTION ( 'NONE',  ( 0.5000000000000045519, -0.8660254037844362651, 0.000000000000000000 ) ) ;
#15018 = CARTESIAN_POINT ( 'NONE',  ( -9.243941288027137659, 79.99999999991588595, -10.56315151873520541 ) ) ;
#15019 = EDGE_CURVE ( 'NONE', #10014, #3518, #16114, .T. ) ;
#15020 = VECTOR ( 'NONE', #6747, 1000.000000000000114 ) ;
#15021 = ORIENTED_EDGE ( 'NONE', *, *, #13963, .T. ) ;
#15022 = DIRECTION ( 'NONE',  ( -0.6048098792058420603, 0.000000000000000000, 0.7963698952214447457 ) ) ;
#15023 = LINE ( 'NONE', #14909, #5109 ) ;
#15024 = DIRECTION ( 'NONE',  ( -0.5000000000000057732, 0.8660254037844352659, 0.000000000000000000 ) ) ;
#15025 = ADVANCED_FACE ( 'NONE', ( #13474 ), #223, .F. ) ;
#15026 = CARTESIAN_POINT ( 'NONE',  ( 82.47279574233218113, 58.94507879694565133, -24.57151460914693075 ) ) ;
#15027 = EDGE_CURVE ( 'NONE', #2860, #13938, #6883, .T. ) ;
#15028 = CARTESIAN_POINT ( 'NONE',  ( -30.00000000000011369, 4.999999999999960920, 7.262422089269331416 ) ) ;
#15029 =( NAMED_UNIT ( * ) SI_UNIT ( $, .STERADIAN. ) SOLID_ANGLE_UNIT ( ) );
#15030 = CYLINDRICAL_SURFACE ( 'NONE', #18097, 5.000000000000002665 ) ;
#15031 = ORIENTED_EDGE ( 'NONE', *, *, #17548, .T. ) ;
#15032 = EDGE_CURVE ( 'NONE', #12266, #16454, #16079, .T. ) ;
#15033 = CARTESIAN_POINT ( 'NONE',  ( 82.19079093293210292, 61.61208316210709057, -25.05535973731833366 ) ) ;
#15034 = CARTESIAN_POINT ( 'NONE',  ( -5.147701114615496287, 45.33223473607662157, -6.247204070674920118 ) ) ;
#15035 = AXIS2_PLACEMENT_3D ( 'NONE', #11098, #12802, #9595 ) ;
#15036 = ORIENTED_EDGE ( 'NONE', *, *, #15084, .F. ) ;
#15037 = CARTESIAN_POINT ( 'NONE',  ( 202.6369081707363193, 24.70788110947296445, -15.42298940083595227 ) ) ;
#15038 = CARTESIAN_POINT ( 'NONE',  ( -3.126021133370410432, 54.92993604554487064, -1.368878731129744564 ) ) ;
#15039 = CARTESIAN_POINT ( 'NONE',  ( -2.078177106580701317, 79.32247413568823902, -8.032153923986145472 ) ) ;
#15040 = FACE_BOUND ( 'NONE', #3249, .T. ) ;
#15041 = CARTESIAN_POINT ( 'NONE',  ( 97.53995344223362451, 199.1648067970725720, 9.117919383928111188 ) ) ;
#15042 = CARTESIAN_POINT ( 'NONE',  ( 219.8340134144083606, 36.08307691593343236, -10.17395310825081189 ) ) ;
#15044 = EDGE_LOOP ( 'NONE', ( #8780, #11688, #3687, #1953, #11196 ) ) ;
#15043 = EDGE_LOOP ( 'NONE', ( #14726, #2937, #15977, #6142, #17785, #11455 ) ) ;
#15045 = ORIENTED_EDGE ( 'NONE', *, *, #2941, .F. ) ;
#15046 = PLANE ( 'NONE',  #4776 ) ;
#15047 = DIRECTION ( 'NONE',  ( 0.5000000000000041078, -0.8660254037844363761, 0.000000000000000000 ) ) ;
#15048 = ORIENTED_EDGE ( 'NONE', *, *, #4110, .T. ) ;
#15049 = ORIENTED_EDGE ( 'NONE', *, *, #10101, .F. ) ;
#15050 = CARTESIAN_POINT ( 'NONE',  ( 4.000000000000000000, -1.759474945355379072, 3.047500000000001652 ) ) ;
#15051 = CARTESIAN_POINT ( 'NONE',  ( 226.1604740915998377, 42.99397083318283563, -12.46964089162983313 ) ) ;
#15052 = CARTESIAN_POINT ( 'NONE',  ( 10.40000000000000568, 0.000000000000000000, 0.000000000000000000 ) ) ;
#15053 = CIRCLE ( 'NONE', #1485, 0.4000000000000001887 ) ;
#15054 = AXIS2_PLACEMENT_3D ( 'NONE', #10377, #3709, #14986 ) ;
#15055 = VERTEX_POINT ( 'NONE', #13264 ) ;
#15056 = LINE ( 'NONE', #16830, #1214 ) ;
#15057 = LINE ( 'NONE', #7067, #14499 ) ;
#15058 = EDGE_LOOP ( 'NONE', ( #9692, #20798, #11623, #16077 ) ) ;
#15059 = DIRECTION ( 'NONE',  ( 0.000000000000000000, 0.000000000000000000, 1.000000000000000000 ) ) ;
#15060 = EDGE_CURVE ( 'NONE', #17374, #14979, #14978, .T. ) ;
#15061 = PLANE ( 'NONE',  #2793 ) ;
#15062 = CARTESIAN_POINT ( 'NONE',  ( -28.49184912364534839, 49.99505663536145050, 0.5228165434693862190 ) ) ;
#15063 = CARTESIAN_POINT ( 'NONE',  ( 205.0443405901917231, 9.676103521955072395, -14.65894010836695038 ) ) ;
#15064 = AXIS2_PLACEMENT_3D ( 'NONE', #13787, #20235, #1065 ) ;
#15065 = FACE_OUTER_BOUND ( 'NONE', #13078, .T. ) ;
#15066 =( BOUNDED_CURVE ( )  B_SPLINE_CURVE ( 3, ( #19780, #13020, #2093, #14931 ),
 .UNSPECIFIED., .F., .F. ) 
 B_SPLINE_CURVE_WITH_KNOTS ( ( 4, 4 ),
 ( 1.772154247585230769, 3.141592653589793116 ),
 .UNSPECIFIED. ) 
 CURVE ( )  GEOMETRIC_REPRESENTATION_ITEM ( )  RATIONAL_B_SPLINE_CURVE ( ( 1.000000000000000000, 0.8497311128276563430, 0.8497311128276563430, 1.000000000000000000 ) ) 
 REPRESENTATION_ITEM ( '' )  );
#15067 = DIRECTION ( 'NONE',  ( -0.8660254037844355990, -0.5000000000000054401, 0.000000000000000000 ) ) ;
#15069 = ORIENTED_EDGE ( 'NONE', *, *, #13192, .F. ) ;
#15068 = ORIENTED_EDGE ( 'NONE', *, *, #12806, .F. ) ;
#15070 = ORIENTED_EDGE ( 'NONE', *, *, #8831, .T. ) ;
#15071 = CARTESIAN_POINT ( 'NONE',  ( 59.50745032656949718, 84.78413469058132534, -15.98776567044169994 ) ) ;
#15072 = VERTEX_POINT ( 'NONE', #13158 ) ;
#15073 = ORIENTED_EDGE ( 'NONE', *, *, #1330, .F. ) ;
#15074 = LINE ( 'NONE', #15283, #1388 ) ;
#15075 = DIRECTION ( 'NONE',  ( 0.4330127018922105830, 0.2499999999999990563, -0.8660254037844432595 ) ) ;
#15076 = ADVANCED_FACE ( 'NONE', ( #15083 ), #20821, .T. ) ;
#15077 = EDGE_LOOP ( 'NONE', ( #12049, #6427, #15877, #8258 ) ) ;
#15078 = LINE ( 'NONE', #16642, #573 ) ;
#15079 = CIRCLE ( 'NONE', #17766, 12.47473710546057823 ) ;
#15080 = CARTESIAN_POINT ( 'NONE',  ( 218.0611881365336444, 9.768376490446161853, -19.34736286182901210 ) ) ;
#15081 = ORIENTED_EDGE ( 'NONE', *, *, #8642, .F. ) ;
#15082 = LINE ( 'NONE', #5182, #14891 ) ;
#15083 = FACE_OUTER_BOUND ( 'NONE', #2534, .T. ) ;
#15084 = EDGE_CURVE ( 'NONE', #18950, #7653, #3932, .T. ) ;
#15085 = EDGE_CURVE ( 'NONE', #7280, #15664, #2568, .T. ) ;
#15086 = PLANE ( 'NONE',  #1756 ) ;
#15087 = LINE ( 'NONE', #6990, #18813 ) ;
#15088 = DIRECTION ( 'NONE',  ( 0.000000000000000000, 0.000000000000000000, -1.000000000000000000 ) ) ;
#15089 = DIRECTION ( 'NONE',  ( -0.5000000000000045519, 0.8660254037844360431, 0.000000000000000000 ) ) ;
#15090 = FACE_OUTER_BOUND ( 'NONE', #5776, .T. ) ;
#15091 = FACE_OUTER_BOUND ( 'NONE', #17738, .T. ) ;
#15092 = ORIENTED_EDGE ( 'NONE', *, *, #9023, .T. ) ;
#15093 = CARTESIAN_POINT ( 'NONE',  ( 79.78989234911249184, 55.62452637193754867, -3.470983589548607640 ) ) ;
#15094 = CIRCLE ( 'NONE', #3893, 5.000000000000008882 ) ;
#15095 = CARTESIAN_POINT ( 'NONE',  ( 206.7427512303946457, 3.748880134758005411, -26.11230899909614678 ) ) ;
#15096 = CARTESIAN_POINT ( 'NONE',  ( 79.19901074457860091, 54.45260783255401549, -20.14565730162479085 ) ) ;
#15098 = ORIENTED_EDGE ( 'NONE', *, *, #16894, .T. ) ;
#15097 = ORIENTED_EDGE ( 'NONE', *, *, #10637, .T. ) ;
#15099 = VERTEX_POINT ( 'NONE', #11563 ) ;
#15100 = CARTESIAN_POINT ( 'NONE',  ( 4.000000000000000000, 0.000000000000000000, 0.000000000000000000 ) ) ;
#15101 = VERTEX_POINT ( 'NONE', #3602 ) ;
#15102 = CARTESIAN_POINT ( 'NONE',  ( 78.05328906524978549, 56.09831538232894843, -3.025823995327162841 ) ) ;
#15103 = CIRCLE ( 'NONE', #8296, 12.47473710546057823 ) ;
#15104 = CARTESIAN_POINT ( 'NONE',  ( -25.51565122030220323, 79.99999999992057553, -8.118105310439162281 ) ) ;
#15105 = DIRECTION ( 'NONE',  ( 0.5000000000000051070, -0.8660254037844359321, 0.000000000000000000 ) ) ;
#15106 = DIRECTION ( 'NONE',  ( 0.5000000000000051070, -0.8660254037844355990, -4.163336342344335178E-17 ) ) ;
#15107 = ORIENTED_EDGE ( 'NONE', *, *, #3317, .F. ) ;
#15108 = EDGE_CURVE ( 'NONE', #8219, #15321, #9971, .T. ) ;
#15109 = EDGE_CURVE ( 'NONE', #1927, #18151, #14053, .T. ) ;
#15110 = CARTESIAN_POINT ( 'NONE',  ( 209.3941655698033912, 12.18747614486167308, -16.05373426534894321 ) ) ;
#15111 = VECTOR ( 'NONE', #19307, 1000.000000000000114 ) ;
#15112 = DIRECTION ( 'NONE',  ( -0.8660254037844357100, -0.5000000000000051070, 0.000000000000000000 ) ) ;
#15113 = CARTESIAN_POINT ( 'NONE',  ( -30.88448036966982002, 64.25000000000000000, 2.547625675852274618 ) ) ;
#15114 = ORIENTED_EDGE ( 'NONE', *, *, #11072, .T. ) ;
#15115 = EDGE_CURVE ( 'NONE', #13758, #13435, #13065, .T. ) ;
#15116 = FACE_OUTER_BOUND ( 'NONE', #7796, .T. ) ;
#15117 = LINE ( 'NONE', #13402, #3722 ) ;
#15118 = EDGE_CURVE ( 'NONE', #7292, #17399, #4918, .T. ) ;
#15119 = DIRECTION ( 'NONE',  ( -1.000000000000000000, -0.000000000000000000, -0.000000000000000000 ) ) ;
#15120 = CARTESIAN_POINT ( 'NONE',  ( -3.212349491796369527, 78.65050410969293182, -6.103909342517296999 ) ) ;
#15121 = ORIENTED_EDGE ( 'NONE', *, *, #20309, .T. ) ;
#15122 = ORIENTED_EDGE ( 'NONE', *, *, #6210, .T. ) ;
#15123 = AXIS2_PLACEMENT_3D ( 'NONE', #11981, #530, #18440 ) ;
#15124 = CARTESIAN_POINT ( 'NONE',  ( 200.8946500511725333, -0.1427288941911568354, -6.310089745291766583 ) ) ;
#15125 = DIRECTION ( 'NONE',  ( 1.000000000000000000, 0.000000000000000000, 0.000000000000000000 ) ) ;
#15126 = AXIS2_PLACEMENT_3D ( 'NONE', #1487, #17710, #19290 ) ;
#15127 = CARTESIAN_POINT ( 'NONE',  ( -33.43925266485176451, 76.85164673649258305, -3.302532775402095222 ) ) ;
#15128 = ADVANCED_FACE ( 'NONE', ( #9302 ), #14426, .T. ) ;
#15129 = CARTESIAN_POINT ( 'NONE',  ( 82.83006403966726339, 60.80631076346477926, -25.10535189848144455 ) ) ;
#15130 = CARTESIAN_POINT ( 'NONE',  ( -26.22900660273689155, 5.421942632918632654, 7.194350572235736152 ) ) ;
#15131 = CARTESIAN_POINT ( 'NONE',  ( 208.8107687779841228, 4.427644383670616079, -14.00000000000005507 ) ) ;
#15132 = ORIENTED_EDGE ( 'NONE', *, *, #8893, .T. ) ;
#15133 = ADVANCED_FACE ( 'NONE', ( #14223 ), #17651, .F. ) ;
#15134 = CARTESIAN_POINT ( 'NONE',  ( 79.20517720625409197, 57.75691248093230001, -23.30626794376461319 ) ) ;
#15135 = AXIS2_PLACEMENT_3D ( 'NONE', #458, #3940, #3521 ) ;
#15136 = CARTESIAN_POINT ( 'NONE',  ( 217.4835782137190279, 9.950099484899608271, -7.237580838290172736 ) ) ;
#15137 = ORIENTED_EDGE ( 'NONE', *, *, #20621, .F. ) ;
#15138 = VECTOR ( 'NONE', #17355, 1000.000000000000227 ) ;
#15139 = CARTESIAN_POINT ( 'NONE',  ( 202.1519482485907986, 25.54804868556654185, -15.42265203330069490 ) ) ;
#15140 = CARTESIAN_POINT ( 'NONE',  ( -4.675102993692958897, 62.87218805480786443, 5.292445494479565582 ) ) ;
#15141 = CARTESIAN_POINT ( 'NONE',  ( 218.2368265400617133, 38.23163736213975028, -12.98880265512657672 ) ) ;
#15142 = AXIS2_PLACEMENT_3D ( 'NONE', #10720, #20371, #16882 ) ;
#15143 = EDGE_CURVE ( 'NONE', #5172, #4848, #20254, .T. ) ;
#15144 = CARTESIAN_POINT ( 'NONE',  ( 204.2542003381767017, 1.796908368366799680, -1.942038651984764996 ) ) ;
#15145 = DIRECTION ( 'NONE',  ( 0.4711304610594120312, -0.8160218955482464454, 0.3348796121709901596 ) ) ;
#15146 = CARTESIAN_POINT ( 'NONE',  ( 208.8107687779841228, 4.427644383670616079, -14.00000000000005507 ) ) ;
#15147 = EDGE_CURVE ( 'NONE', #20014, #15175, #3910, .T. ) ;
#15149 = ORIENTED_EDGE ( 'NONE', *, *, #1084, .F. ) ;
#15148 = ORIENTED_EDGE ( 'NONE', *, *, #14874, .T. ) ;
#15150 = ORIENTED_EDGE ( 'NONE', *, *, #17677, .T. ) ;
#15151 = LINE ( 'NONE', #3988, #18312 ) ;
#15152 = CARTESIAN_POINT ( 'NONE',  ( 229.1391642386170133, 37.18176902604204770, -16.42873025640184537 ) ) ;
#15153 = ORIENTED_EDGE ( 'NONE', *, *, #8456, .F. ) ;
#15154 = CARTESIAN_POINT ( 'NONE',  ( 195.0976485947789456, 3.402328959064704783, -12.53629070788332278 ) ) ;
#15155 = B_SPLINE_CURVE_WITH_KNOTS ( 'NONE', 3,
 ( #18752, #10672, #2745, #15584 ),
 .UNSPECIFIED., .F., .F.,
 ( 4, 4 ),
 ( 6.222750521083429372E-05, 0.0007348782972656951393 ),
 .UNSPECIFIED. ) ;
#15156 = LINE ( 'NONE', #18415, #8132 ) ;
#15157 = CARTESIAN_POINT ( 'NONE',  ( 227.1472425980001333, 40.30537175372559489, -10.17395310825081012 ) ) ;
#15158 = ORIENTED_EDGE ( 'NONE', *, *, #15439, .F. ) ;
#15159 = EDGE_CURVE ( 'NONE', #437, #15357, #5716, .T. ) ;
#15160 = DIRECTION ( 'NONE',  ( 1.000000000000000000, 0.000000000000000000, 0.000000000000000000 ) ) ;
#15161 = CIRCLE ( 'NONE', #11403, 12.47473710546057823 ) ;
#15162 = LINE ( 'NONE', #8557, #16485 ) ;
#15163 = EDGE_LOOP ( 'NONE', ( #12051, #19645, #16414, #18701 ) ) ;
#15164 = LINE ( 'NONE', #19791, #6715 ) ;
#15165 = EDGE_CURVE ( 'NONE', #2805, #8118, #8195, .T. ) ;
#15166 = DIRECTION ( 'NONE',  ( 0.5000000000000045519, -0.8660254037844360431, 0.000000000000000000 ) ) ;
#15167 = CARTESIAN_POINT ( 'NONE',  ( -30.91092412438536385, 50.20590819142025651, -10.00467867777946473 ) ) ;
#15168 = CARTESIAN_POINT ( 'NONE',  ( -16.66469718191209282, 20.06594084399080558, 12.48650452048989479 ) ) ;
#15169 = EDGE_LOOP ( 'NONE', ( #14902, #1681 ) ) ;
#15170 = DIRECTION ( 'NONE',  ( -0.5000000000000026645, 0.8660254037844370423, 0.000000000000000000 ) ) ;
#15171 = LINE ( 'NONE', #18118, #5611 ) ;
#15172 = CIRCLE ( 'NONE', #7689, 4.000000000000000000 ) ;
#15173 = ADVANCED_BREP_SHAPE_REPRESENTATION ( '', ( #3293, #18233 ), #6025 ) ;
#15175 = VERTEX_POINT ( 'NONE', #9016 ) ;
#15174 = ORIENTED_EDGE ( 'NONE', *, *, #5494, .T. ) ;
#15176 = CARTESIAN_POINT ( 'NONE',  ( 59.16309583933880845, 85.04882181297647037, -15.26077928376918358 ) ) ;
#15177 = ORIENTED_EDGE ( 'NONE', *, *, #6378, .T. ) ;
#15178 = VERTEX_POINT ( 'NONE', #867 ) ;
#15179 = DIRECTION ( 'NONE',  ( 0.5000000000000044409, -0.8660254037844360431, -4.006172263299080068E-16 ) ) ;
#15180 = CARTESIAN_POINT ( 'NONE',  ( -4.701390418375632763, 64.25000000000000000, 5.347094680480811490 ) ) ;
#15181 = ORIENTED_EDGE ( 'NONE', *, *, #11093, .F. ) ;
#15182 = CARTESIAN_POINT ( 'NONE',  ( 212.9776690748797989, 18.38041077556222191, -19.29168348739316130 ) ) ;
#15183 = CARTESIAN_POINT ( 'NONE',  ( 218.0822574325961511, 10.03814007800654551, -19.43577154980806299 ) ) ;
#15184 = ORIENTED_EDGE ( 'NONE', *, *, #6158, .F. ) ;
#15185 = CIRCLE ( 'NONE', #20893, 4.057500000000000107 ) ;
#15186 = PRODUCT_DEFINITION_SHAPE ( 'NONE', 'NONE',  #7172 ) ;
#15187 = CARTESIAN_POINT ( 'NONE',  ( 213.2500461588270468, 13.88262057910513825, -23.06309126349817618 ) ) ;
#15188 = FACE_OUTER_BOUND ( 'NONE', #17524, .T. ) ;
#15189 = VECTOR ( 'NONE', #12228, 1000.000000000000114 ) ;
#15190 = FACE_OUTER_BOUND ( 'NONE', #11141, .T. ) ;
#15191 = DIRECTION ( 'NONE',  ( 0.06808332454812035528, -0.1179237772655450517, 0.9906859460363316439 ) ) ;
#15192 = CARTESIAN_POINT ( 'NONE',  ( 218.0936335691685599, 36.96614847458959474, -11.35524774226742828 ) ) ;
#15193 = VERTEX_POINT ( 'NONE', #18677 ) ;
#15194 = CARTESIAN_POINT ( 'NONE',  ( 216.6298941398503359, 15.83397672076898566, -14.01558723443205068 ) ) ;
#15195 = DIRECTION ( 'NONE',  ( -1.000000000000000000, 0.000000000000000000, -0.000000000000000000 ) ) ;
#15196 = CARTESIAN_POINT ( 'NONE',  ( 214.8665333410018263, 15.34694915066777909, -8.609703802792745719 ) ) ;
#15197 = ORIENTED_EDGE ( 'NONE', *, *, #14844, .T. ) ;
#15198 = LINE ( 'NONE', #15306, #14940 ) ;
#15199 = VERTEX_POINT ( 'NONE', #15515 ) ;
#15200 = AXIS2_PLACEMENT_3D ( 'NONE', #8907, #16972, #13589 ) ;
#15201 = DIRECTION ( 'NONE',  ( -0.000000000000000000, -0.000000000000000000, 1.000000000000000000 ) ) ;
#15202 = FACE_OUTER_BOUND ( 'NONE', #14515, .T. ) ;
#15204 = VERTEX_POINT ( 'NONE', #4155 ) ;
#15203 = ORIENTED_EDGE ( 'NONE', *, *, #19914, .T. ) ;
#15205 = ADVANCED_FACE ( 'NONE', ( #8915 ), #18362, .F. ) ;
#15206 = DIRECTION ( 'NONE',  ( 1.000000000000000000, 0.000000000000000000, 0.000000000000000000 ) ) ;
#15207 = CARTESIAN_POINT ( 'NONE',  ( 212.8527399996651752, 6.761277556564890823, -3.125199447383528284 ) ) ;
#15208 = ORIENTED_EDGE ( 'NONE', *, *, #11420, .F. ) ;
#15209 = CARTESIAN_POINT ( 'NONE',  ( 76.25855100882986903, 53.63624723668596772, -18.84667540378509898 ) ) ;
#15210 = CARTESIAN_POINT ( 'NONE',  ( -18.59213065175719493, 79.99957779460252993, -12.37049764041025135 ) ) ;
#15211 = CARTESIAN_POINT ( 'NONE',  ( 206.7852296553355131, 3.258198825955272326, -1.053683606938436768 ) ) ;
#15212 = DIRECTION ( 'NONE',  ( -0.5000000000000045519, 0.8660254037844359321, 0.000000000000000000 ) ) ;
#15213 = ORIENTED_EDGE ( 'NONE', *, *, #14323, .F. ) ;
#15214 = VECTOR ( 'NONE', #18789, 1000.000000000000000 ) ;
#15215 = CARTESIAN_POINT ( 'NONE',  ( 221.5793113145849134, 32.44228390914006610, -15.46846178913030201 ) ) ;
#15216 = ADVANCED_FACE ( 'NONE', ( #15202 ), #16766, .F. ) ;
#15217 = CARTESIAN_POINT ( 'NONE',  ( 82.49529059433407951, 181.0703347563770365, 6.000000000000009770 ) ) ;
#15218 = FACE_OUTER_BOUND ( 'NONE', #18754, .T. ) ;
#15219 = ORIENTED_EDGE ( 'NONE', *, *, #2834, .T. ) ;
#15220 = CARTESIAN_POINT ( 'NONE',  ( 159.9952905943348469, 46.83639716978958489, -29.00000000000006750 ) ) ;
#15221 = CARTESIAN_POINT ( 'NONE',  ( -3.510843195177425713, 80.00000000000000000, 0.5205403966592460074 ) ) ;
#15222 = CARTESIAN_POINT ( 'NONE',  ( 196.2242827900706175, 4.229814195430575907, -19.53076827296950668 ) ) ;
#15223 = DIRECTION ( 'NONE',  ( 0.3878556453522086223, -0.6717856837524379676, 0.6310879443260591914 ) ) ;
#15224 = EDGE_CURVE ( 'NONE', #1288, #13189, #6258, .T. ) ;
#15226 = ORIENTED_EDGE ( 'NONE', *, *, #5617, .F. ) ;
#15225 = EDGE_LOOP ( 'NONE', ( #2884, #9038, #4966 ) ) ;
#15227 = EDGE_LOOP ( 'NONE', ( #15380, #20868, #14374, #11339, #19296, #2329 ) ) ;
#15228 = VECTOR ( 'NONE', #14643, 1000.000000000000000 ) ;
#15229 = ADVANCED_FACE ( 'NONE', ( #15413 ), #9983, .T. ) ;
#15230 = DIRECTION ( 'NONE',  ( 0.8660254037844357100, 0.5000000000000053291, 0.000000000000000000 ) ) ;
#15231 = CARTESIAN_POINT ( 'NONE',  ( 54.18022169236989072, 134.1134727143927989, 41.00000000000001421 ) ) ;
#15232 = DIRECTION ( 'NONE',  ( 0.8660254037844370423, 0.5000000000000026645, -0.000000000000000000 ) ) ;
#15233 = DIRECTION ( 'NONE',  ( 0.000000000000000000, 0.5000000000000024425, 0.8660254037844372643 ) ) ;
#15234 = CARTESIAN_POINT ( 'NONE',  ( -28.49993446417160570, 8.570804147430656883, -0.3390835457399271058 ) ) ;
#15235 = CARTESIAN_POINT ( 'NONE',  ( 184.9952905943349606, 3.535126980567713240, 0.9999999999999876765 ) ) ;
#15236 = ORIENTED_EDGE ( 'NONE', *, *, #4483, .T. ) ;
#15237 = ADVANCED_FACE ( 'NONE', ( #3829 ), #6999, .F. ) ;
#15238 = CARTESIAN_POINT ( 'NONE',  ( 77.17349984701002086, 54.87731286059718627, -20.67167348712315444 ) ) ;
#15239 = CARTESIAN_POINT ( 'NONE',  ( 60.23610500267373169, 84.22369677626844009, -17.09587939145292523 ) ) ;
#15240 = VECTOR ( 'NONE', #6613, 1000.000000000000114 ) ;
#15241 = ORIENTED_EDGE ( 'NONE', *, *, #8626, .F. ) ;
#15242 = CARTESIAN_POINT ( 'NONE',  ( 203.1748089687253582, 24.07645447784576831, -14.75390691332407300 ) ) ;
#15243 = CARTESIAN_POINT ( 'NONE',  ( 205.8894739819445761, 2.741034046794848855, -25.34310559273324159 ) ) ;
#15244 = DIRECTION ( 'NONE',  ( -0.000000000000000000, 1.000000000000000000, -0.000000000000000000 ) ) ;
#15245 = EDGE_CURVE ( 'NONE', #8118, #7107, #17129, .T. ) ;
#15246 = DIRECTION ( 'NONE',  ( -0.8660254037844354880, -0.5000000000000055511, 0.000000000000000000 ) ) ;
#15247 = CARTESIAN_POINT ( 'NONE',  ( 96.94205509780233854, 198.6678179064276435, 10.35076502982056113 ) ) ;
#15248 = CARTESIAN_POINT ( 'NONE',  ( 219.3753053876406511, 36.25973415479045059, -17.38313153181858084 ) ) ;
#15250 = ORIENTED_EDGE ( 'NONE', *, *, #422, .F. ) ;
#15249 = VERTEX_POINT ( 'NONE', #15311 ) ;
#15251 = ORIENTED_EDGE ( 'NONE', *, *, #15754, .F. ) ;
#15252 = FACE_OUTER_BOUND ( 'NONE', #10165, .T. ) ;
#15253 = CARTESIAN_POINT ( 'NONE',  ( 203.2584098944515461, 1.737194726502687470, -24.64792178047091653 ) ) ;
#15254 = AXIS2_PLACEMENT_3D ( 'NONE', #16823, #19991, #708 ) ;
#15255 = EDGE_CURVE ( 'NONE', #16063, #13880, #7219, .T. ) ;
#15256 = ORIENTED_EDGE ( 'NONE', *, *, #5888, .T. ) ;
#15257 = DIRECTION ( 'NONE',  ( 0.000000000000000000, -1.000000000000000000, 0.000000000000000000 ) ) ;
#15258 = LINE ( 'NONE', #10016, #19651 ) ;
#15259 = DIRECTION ( 'NONE',  ( -0.8645602258681718277, -0.4991540791356397500, -0.05814482891046558743 ) ) ;
#15260 = ORIENTED_EDGE ( 'NONE', *, *, #583, .F. ) ;
#15261 = PLANE ( 'NONE',  #11692 ) ;
#15262 = DIRECTION ( 'NONE',  ( -0.5000000000000045519, 0.8660254037844360431, 0.000000000000000000 ) ) ;
#15263 = AXIS2_PLACEMENT_3D ( 'NONE', #1017, #7356, #11944 ) ;
#15264 = EDGE_CURVE ( 'NONE', #10920, #16780, #20776, .T. ) ;
#15265 = ORIENTED_EDGE ( 'NONE', *, *, #7824, .T. ) ;
#15266 = AXIS2_PLACEMENT_3D ( 'NONE', #8565, #17053, #934 ) ;
#15267 = EDGE_CURVE ( 'NONE', #15362, #5527, #18493, .T. ) ;
#15268 = PLANE ( 'NONE',  #5376 ) ;
#15269 = DIRECTION ( 'NONE',  ( 0.000000000000000000, -6.938893903907177533E-18, -1.000000000000000000 ) ) ;
#15270 = CARTESIAN_POINT ( 'NONE',  ( -27.10521411282678628, 51.35483501200679513, -5.980665530051757273 ) ) ;
#15271 = CARTESIAN_POINT ( 'NONE',  ( 203.7983348743963461, 8.956721786528811791, -25.65046807331631129 ) ) ;
#15272 = EDGE_CURVE ( 'NONE', #5028, #8582, #6244, .T. ) ;
#15273 = VERTEX_POINT ( 'NONE', #7639 ) ;
#15274 = FACE_OUTER_BOUND ( 'NONE', #10138, .T. ) ;
#15275 = DIRECTION ( 'NONE',  ( -0.8944271909999147452, 0.000000000000000000, 0.4472135954999602592 ) ) ;
#15277 = VERTEX_POINT ( 'NONE', #3185 ) ;
#15276 = VERTEX_POINT ( 'NONE', #12733 ) ;
#15278 = VECTOR ( 'NONE', #15835, 1000.000000000000227 ) ;
#15279 = CARTESIAN_POINT ( 'NONE',  ( 62.22363694231594167, 78.39636059616459818, -14.27859498331829080 ) ) ;
#15280 = CIRCLE ( 'NONE', #5081, 5.000000000000008882 ) ;
#15281 = VERTEX_POINT ( 'NONE', #4361 ) ;
#15282 = VERTEX_POINT ( 'NONE', #14022 ) ;
#15283 = CARTESIAN_POINT ( 'NONE',  ( -14.99999999999999645, 5.000000000000000000, 30.00000000000000000 ) ) ;
#15284 = CARTESIAN_POINT ( 'NONE',  ( 5.000000000000004441, 4.685197434473814759, -6.938893903907228378E-15 ) ) ;
#15285 = EDGE_CURVE ( 'NONE', #11917, #7471, #6041, .T. ) ;
#15286 = CONICAL_SURFACE ( 'NONE', #18651, 4.999999999999944933, 1.566852922939436121 ) ;
#15287 = EDGE_LOOP ( 'NONE', ( #13480, #5102, #7210, #20766 ) ) ;
#15288 = ORIENTED_EDGE ( 'NONE', *, *, #5764, .F. ) ;
#15289 = CARTESIAN_POINT ( 'NONE',  ( 32.36389338619004263, 157.9004617752989930, 4.000000000000000000 ) ) ;
#15290 = VERTEX_POINT ( 'NONE', #1495 ) ;
#15291 = EDGE_CURVE ( 'NONE', #8683, #13569, #15802, .T. ) ;
#15292 = DIRECTION ( 'NONE',  ( 0.8660254037844380415, 0.5000000000000014433, 0.000000000000000000 ) ) ;
#15293 = VECTOR ( 'NONE', #5048, 1000.000000000000000 ) ;
#15294 = DIRECTION ( 'NONE',  ( 0.000000000000000000, 0.000000000000000000, -1.000000000000000000 ) ) ;
#15295 = VECTOR ( 'NONE', #15889, 1000.000000000000227 ) ;
#15296 = CYLINDRICAL_SURFACE ( 'NONE', #17232, 7.960520131757808038 ) ;
#15297 = DIRECTION ( 'NONE',  ( 1.000000000000000000, 0.000000000000000000, 0.000000000000000000 ) ) ;
#15298 = VECTOR ( 'NONE', #17059, 1000.000000000000000 ) ;
#15299 = LINE ( 'NONE', #2555, #15324 ) ;
#15300 = DIRECTION ( 'NONE',  ( -0.5000000000000054401, 0.8660254037844354880, -0.000000000000000000 ) ) ;
#15301 = CARTESIAN_POINT ( 'NONE',  ( 34.99529059433362477, 263.3427481158986438, -28.99999999999998934 ) ) ;
#15302 = CARTESIAN_POINT ( 'NONE',  ( -28.18912803645524789, 76.46633113979225982, 2.786148689273399981 ) ) ;
#15303 = DIRECTION ( 'NONE',  ( 0.000000000000000000, 0.000000000000000000, -1.000000000000000000 ) ) ;
#15304 = CARTESIAN_POINT ( 'NONE',  ( 195.3983247169765320, 4.106973660946812821, -14.97708215022677791 ) ) ;
#15305 = EDGE_LOOP ( 'NONE', ( #2611, #19095, #2482, #10698 ) ) ;
#15306 = CARTESIAN_POINT ( 'NONE',  ( 200.0522846737218856, -0.6290687716183213096, -5.585956497639848806 ) ) ;
#15307 = AXIS2_PLACEMENT_3D ( 'NONE', #17041, #2519, #20311 ) ;
#15308 = ORIENTED_EDGE ( 'NONE', *, *, #15019, .T. ) ;
#15309 = DIRECTION ( 'NONE',  ( -0.8660254037844364872, -0.5000000000000041078, 0.000000000000000000 ) ) ;
#15310 = AXIS2_PLACEMENT_3D ( 'NONE', #29, #9654, #17737 ) ;
#15311 = CARTESIAN_POINT ( 'NONE',  ( 216.7438708388689292, 9.007822994031293717, -21.66653917424403986 ) ) ;
#15312 = VECTOR ( 'NONE', #20178, 1000.000000000000227 ) ;
#15313 = DIRECTION ( 'NONE',  ( 0.000000000000000000, 0.000000000000000000, 1.000000000000000000 ) ) ;
#15314 = APPLICATION_CONTEXT ( 'automotive_design' ) ;
#15315 = DIRECTION ( 'NONE',  ( -0.8660254037844370423, -0.5000000000000026645, 0.000000000000000000 ) ) ;
#15316 = ORIENTED_EDGE ( 'NONE', *, *, #7586, .T. ) ;
#15317 = CARTESIAN_POINT ( 'NONE',  ( 81.31407792830592030, 61.42543535009416900, -25.00296011795888518 ) ) ;
#15318 = CARTESIAN_POINT ( 'NONE',  ( -16.52214040532013684, 80.00000000000014211, -12.49180211257053230 ) ) ;
#15319 = CARTESIAN_POINT ( 'NONE',  ( 220.8589169312680838, 34.30789195187642093, -17.68583624946730737 ) ) ;
#15320 = DIRECTION ( 'NONE',  ( 0.6634139481689435014, 0.3830222215594971114, 0.6427876096865291489 ) ) ;
#15321 = VERTEX_POINT ( 'NONE', #11251 ) ;
#15322 = DIRECTION ( 'NONE',  ( 0.8660254037844360431, 0.5000000000000044409, -5.976026924694053325E-17 ) ) ;
#15323 = AXIS2_PLACEMENT_3D ( 'NONE', #14837, #14938, #6320 ) ;
#15324 = VECTOR ( 'NONE', #11992, 1000.000000000000114 ) ;
#15325 = CARTESIAN_POINT ( 'NONE',  ( 61.99529059433388767, 216.5773763115390693, -28.99999999999998934 ) ) ;
#15326 = ADVANCED_FACE ( 'NONE', ( #7942 ), #16796, .T. ) ;
#15327 = DIRECTION ( 'NONE',  ( -0.5000000000000054401, 0.8660254037844354880, -0.000000000000000000 ) ) ;
#15328 = ORIENTED_EDGE ( 'NONE', *, *, #8076, .T. ) ;
#15329 = LINE ( 'NONE', #12232, #18630 ) ;
#15330 = DIRECTION ( 'NONE',  ( 0.5000000000000054401, -0.8660254037844354880, -2.220446049250312834E-16 ) ) ;
#15331 = CARTESIAN_POINT ( 'NONE',  ( 229.0913681223419474, 37.91751346033715464, -10.82724490084735791 ) ) ;
#15332 = DIRECTION ( 'NONE',  ( 0.5000000000000045519, -0.8660254037844360431, -4.006172263299080561E-16 ) ) ;
#15334 = VERTEX_POINT ( 'NONE', #17401 ) ;
#15333 = ORIENTED_EDGE ( 'NONE', *, *, #13010, .T. ) ;
#15335 = EDGE_LOOP ( 'NONE', ( #16186, #11321, #4790, #18215 ) ) ;
#15336 = FACE_OUTER_BOUND ( 'NONE', #20667, .T. ) ;
#15337 = LINE ( 'NONE', #4181, #16296 ) ;
#15338 = PLANE ( 'NONE',  #20208 ) ;
#15339 = AXIS2_PLACEMENT_3D ( 'NONE', #2790, #17414, #2585 ) ;
#15340 = CIRCLE ( 'NONE', #17350, 6.500000000000047962 ) ;
#15341 = CARTESIAN_POINT ( 'NONE',  ( 81.34596348373698049, 55.15737503394385755, -22.61349628177035243 ) ) ;
#15342 = CARTESIAN_POINT ( 'NONE',  ( -28.40887611229263143, 6.478901333902477688, -1.571843926571936612 ) ) ;
#15343 = CYLINDRICAL_SURFACE ( 'NONE', #10633, 13.50000000000000711 ) ;
#15344 = ORIENTED_EDGE ( 'NONE', *, *, #723, .T. ) ;
#15345 = CARTESIAN_POINT ( 'NONE',  ( 81.19763523304686714, 64.84546557366820707, -25.50103675175597573 ) ) ;
#15346 = CARTESIAN_POINT ( 'NONE',  ( 58.69853696180994262, 85.40577002866142209, -13.78609211422347869 ) ) ;
#15347 = EDGE_CURVE ( 'NONE', #3183, #18356, #1230, .T. ) ;
#15348 = ORIENTED_EDGE ( 'NONE', *, *, #5613, .T. ) ;
#15349 = EDGE_CURVE ( 'NONE', #305, #1221, #19487, .T. ) ;
#15350 = CARTESIAN_POINT ( 'NONE',  ( 201.8234976231972553, 26.52995303002162331, -14.00000000000004619 ) ) ;
#15351 = LINE ( 'NONE', #10749, #14157 ) ;
#15352 = AXIS2_PLACEMENT_3D ( 'NONE', #7430, #20374, #1096 ) ;
#15353 = DIRECTION ( 'NONE',  ( 1.000000000000000000, 0.000000000000000000, 0.000000000000000000 ) ) ;
#15354 = CARTESIAN_POINT ( 'NONE',  ( 226.2813836805521248, 42.78454928199521845, -16.00491213559311277 ) ) ;
#15355 = CARTESIAN_POINT ( 'NONE',  ( 209.4907977912995136, 12.24326678395483725, -12.83329734752810225 ) ) ;
#15357 = VERTEX_POINT ( 'NONE', #10932 ) ;
#15356 = ORIENTED_EDGE ( 'NONE', *, *, #11093, .T. ) ;
#15358 = ORIENTED_EDGE ( 'NONE', *, *, #15371, .T. ) ;
#15359 = VERTEX_POINT ( 'NONE', #12638 ) ;
#15360 = CARTESIAN_POINT ( 'NONE',  ( 5.000000000000000000, -3.513898075855360847, -2.028749999999992504 ) ) ;
#15361 = LINE ( 'NONE', #399, #7480 ) ;
#15362 = VERTEX_POINT ( 'NONE', #2881 ) ;
#15363 = VERTEX_POINT ( 'NONE', #15822 ) ;
#15364 = SURFACE_STYLE_FILL_AREA ( #3884 ) ;
#15365 = PRODUCT ( 'MAS-328', 'MAS-328', '', ( #10607 ) ) ;
#15366 = CARTESIAN_POINT ( 'NONE',  ( 220.9456214122823212, 32.02636062774785586, -11.31761084191181510 ) ) ;
#15367 = CARTESIAN_POINT ( 'NONE',  ( 227.6096221818959009, 40.48397271309900702, -10.44704522969157345 ) ) ;
#15368 = CARTESIAN_POINT ( 'NONE',  ( 5.759474945355412601, 0.000000000000000000, 0.000000000000000000 ) ) ;
#15369 = PRODUCT_DEFINITION ( 'UNKNOWN', '', #16886, #2606 ) ;
#15370 = DIRECTION ( 'NONE',  ( 0.5000000000000054401, -0.8660254037844354880, 0.000000000000000000 ) ) ;
#15371 = EDGE_CURVE ( 'NONE', #12727, #15665, #15724, .T. ) ;
#15372 = CARTESIAN_POINT ( 'NONE',  ( 205.0584722627656049, 9.507252542736225109, -1.872710068124171290 ) ) ;
#15373 = EDGE_CURVE ( 'NONE', #15175, #4315, #20670, .T. ) ;
#15374 = CARTESIAN_POINT ( 'NONE',  ( 49.86389338619021316, 127.5895726428436205, -12.50000000000000000 ) ) ;
#15375 = CARTESIAN_POINT ( 'NONE',  ( -18.57755300701755274, 49.50817056232955338, -12.23824556917615780 ) ) ;
#15376 = FACE_OUTER_BOUND ( 'NONE', #9832, .T. ) ;
#15377 = EDGE_CURVE ( 'NONE', #14697, #15381, #17463, .T. ) ;
#15378 = CARTESIAN_POINT ( 'NONE',  ( 226.9451417009221075, 41.63488666678334482, -16.94731950718123059 ) ) ;
#15379 = LINE ( 'NONE', #12291, #19825 ) ;
#15381 = VERTEX_POINT ( 'NONE', #17507 ) ;
#15380 = ORIENTED_EDGE ( 'NONE', *, *, #9028, .F. ) ;
#15382 = VERTEX_POINT ( 'NONE', #2983 ) ;
#15383 = VECTOR ( 'NONE', #121, 1000.000000000000000 ) ;
#15384 = CARTESIAN_POINT ( 'NONE',  ( 202.4756851904152484, 24.94598553735895763, -12.50985653407239795 ) ) ;
#15385 = VECTOR ( 'NONE', #1871, 1000.000000000000000 ) ;
#15386 = CARTESIAN_POINT ( 'NONE',  ( 63.20289482801889847, 77.81544268501482975, -16.80222038511762506 ) ) ;
#15387 = ORIENTED_EDGE ( 'NONE', *, *, #19141, .T. ) ;
#15388 = EDGE_CURVE ( 'NONE', #5897, #10313, #14441, .T. ) ;
#15389 = EDGE_LOOP ( 'NONE', ( #16793, #4519 ) ) ;
#15390 = CYLINDRICAL_SURFACE ( 'NONE', #25, 12.47473710546057646 ) ;
#15391 = CARTESIAN_POINT ( 'NONE',  ( 44.99529059433372424, 246.0222400402097946, -13.99999999999997513 ) ) ;
#15392 = VERTEX_POINT ( 'NONE', #9836 ) ;
#15393 = EDGE_LOOP ( 'NONE', ( #5016, #13954, #17656, #209 ) ) ;
#15394 = LINE ( 'NONE', #10257, #1951 ) ;
#15395 = ADVANCED_FACE ( 'NONE', ( #3381 ), #16222, .T. ) ;
#15396 = CARTESIAN_POINT ( 'NONE',  ( 58.37797649651341203, 276.8427481158987007, -0.9999999999999826805 ) ) ;
#15397 = DIRECTION ( 'NONE',  ( 0.5000000000000052180, -0.8660254037844355990, 0.000000000000000000 ) ) ;
#15398 = PLANE ( 'NONE',  #10104 ) ;
#15399 = EDGE_CURVE ( 'NONE', #3183, #10792, #9939, .T. ) ;
#15400 = DIRECTION ( 'NONE',  ( 0.000000000000000000, 0.9718000864392509763, 0.2358062594518311739 ) ) ;
#15401 = DIRECTION ( 'NONE',  ( 0.000000000000000000, 0.7332630167743484639, 0.6799451067777320112 ) ) ;
#15402 = DIRECTION ( 'NONE',  ( 0.000000000000000000, -1.000000000000000000, 0.000000000000000000 ) ) ;
#15403 = ORIENTED_EDGE ( 'NONE', *, *, #19591, .T. ) ;
#15404 = CARTESIAN_POINT ( 'NONE',  ( -27.70576433140186268, 72.30161019874638839, 4.406123080992779606 ) ) ;
#15405 = DIRECTION ( 'NONE',  ( -0.2483788854153066994, -0.1434016163555488221, -0.9579895123154877901 ) ) ;
#15406 = CARTESIAN_POINT ( 'NONE',  ( 212.8960219706529813, 6.786266414165766925, -3.025685634606239294 ) ) ;
#15407 = EDGE_LOOP ( 'NONE', ( #14692, #20647, #3876, #830, #16313 ) ) ;
#15408 = CARTESIAN_POINT ( 'NONE',  ( 81.67521804894028037, 59.84799745248609071, -0.5475991497997765300 ) ) ;
#15409 = ADVANCED_FACE ( 'NONE', ( #16431 ), #4971, .F. ) ;
#15410 = ORIENTED_EDGE ( 'NONE', *, *, #20162, .F. ) ;
#15411 = PLANE ( 'NONE',  #1711 ) ;
#15412 = VECTOR ( 'NONE', #6690, 1000.000000000000000 ) ;
#15413 = FACE_OUTER_BOUND ( 'NONE', #15058, .T. ) ;
#15414 = DIRECTION ( 'NONE',  ( 1.000000000000000000, 0.000000000000000000, 0.000000000000000000 ) ) ;
#15415 = ADVANCED_FACE ( 'NONE', ( #8462 ), #4876, .F. ) ;
#15416 = LINE ( 'NONE', #7320, #8583 ) ;
#15417 = VERTEX_POINT ( 'NONE', #5278 ) ;
#15418 = DIRECTION ( 'NONE',  ( -0.5000000000000051070, 0.8660254037844359321, -0.000000000000000000 ) ) ;
#15419 = CARTESIAN_POINT ( 'NONE',  ( 201.7020968622623798, 0.3234507395478347092, -5.321846656828017608 ) ) ;
#15420 = DIRECTION ( 'NONE',  ( 0.000000000000000000, -0.9929900419787565102, -0.1181980394550916635 ) ) ;
#15421 = LINE ( 'NONE', #4049, #14672 ) ;
#15422 = AXIS2_PLACEMENT_3D ( 'NONE', #6484, #13086, #11282 ) ;
#15423 = EDGE_CURVE ( 'NONE', #4996, #513, #3891, .T. ) ;
#15424 = DIRECTION ( 'NONE',  ( -0.8660254037844354880, -0.5000000000000055511, 0.000000000000000000 ) ) ;
#15425 = CARTESIAN_POINT ( 'NONE',  ( 34.99529059433359635, 263.3427481158985870, -22.00000000000000355 ) ) ;
#15426 = ORIENTED_EDGE ( 'NONE', *, *, #16298, .T. ) ;
#15427 = CARTESIAN_POINT ( 'NONE',  ( 38.17255043510031953, 120.8395726428435637, -12.49999999999999822 ) ) ;
#15428 = CARTESIAN_POINT ( 'NONE',  ( -4.318268741000043320, 72.07281518094384865, 4.467622400254039228 ) ) ;
#15429 = B_SPLINE_CURVE_WITH_KNOTS ( 'NONE', 3,
 ( #2163, #8616, #15113, #569, #12988, #16262, #1743, #13194, #14696, #151, #20269, #10510, #18481, #10401 ),
 .UNSPECIFIED., .F., .F.,
 ( 4, 2, 2, 2, 2, 2, 4 ),
 ( 0.000000000000000000, 0.001404842194932282235, 0.002107263292398423027, 0.002809684389864564470, 0.003512105487330705912, 0.004214526584796846054, 0.005619368779729120265 ),
 .UNSPECIFIED. ) ;
#15430 = DIRECTION ( 'NONE',  ( -0.5000000000000054401, 0.8660254037844354880, -0.000000000000000000 ) ) ;
#15431 = CARTESIAN_POINT ( 'NONE',  ( 216.2517163971578782, 7.460585314318640471, -14.00000000000005507 ) ) ;
#15432 = B_SPLINE_CURVE_WITH_KNOTS ( 'NONE', 3,
 ( #5307, #8819, #7013, #357 ),
 .UNSPECIFIED., .F., .F.,
 ( 4, 4 ),
 ( 5.324950961081164366E-05, 0.0009072352475936213290 ),
 .UNSPECIFIED. ) ;
#15434 = ORIENTED_EDGE ( 'NONE', *, *, #16294, .T. ) ;
#15433 = ORIENTED_EDGE ( 'NONE', *, *, #6942, .T. ) ;
#15435 = EDGE_LOOP ( 'NONE', ( #14072, #5104 ) ) ;
#15436 = DIRECTION ( 'NONE',  ( 0.000000000000000000, 0.5000000000000018874, 0.8660254037844374864 ) ) ;
#15437 = VERTEX_POINT ( 'NONE', #8144 ) ;
#15438 = CARTESIAN_POINT ( 'NONE',  ( 65.63317740310760939, 80.05417074498873831, -21.46107424520661411 ) ) ;
#15439 = EDGE_CURVE ( 'NONE', #13569, #8683, #5609, .T. ) ;
#15440 = AXIS2_PLACEMENT_3D ( 'NONE', #10940, #7747, #6250 ) ;
#15441 = CARTESIAN_POINT ( 'NONE',  ( -28.43238653473407496, 8.661473207178586264, 1.341288757007061516 ) ) ;
#15442 = AXIS2_PLACEMENT_3D ( 'NONE', #756, #10372, #13478 ) ;
#15443 = SHAPE_REPRESENTATION_RELATIONSHIP ( 'NONE' , 'NONE' ,  #20602, #10594 ) ;
#15444 = CARTESIAN_POINT ( 'NONE',  ( 229.6690045275718717, 36.91701785817784298, -12.98880265512672416 ) ) ;
#15445 = ORIENTED_EDGE ( 'NONE', *, *, #2145, .F. ) ;
#15446 = CARTESIAN_POINT ( 'NONE',  ( 218.3424216846280501, 38.25465940752314253, -12.57085682670540194 ) ) ;
#15447 = DIRECTION ( 'NONE',  ( 0.000000000000000000, 0.000000000000000000, -1.000000000000000000 ) ) ;
#15448 = EDGE_LOOP ( 'NONE', ( #12824, #13433, #1314, #8869 ) ) ;
#15449 = CARTESIAN_POINT ( 'NONE',  ( 229.6243373519787099, 36.99438367573579001, -12.60011953066312529 ) ) ;
#15450 = CARTESIAN_POINT ( 'NONE',  ( 198.2231302758563913, -1.169925316738297028, -11.16899820387730635 ) ) ;
#15451 = CLOSED_SHELL ( 'NONE', ( #10590, #4195, #1764, #6828, #7726, #9885, #3768, #18434, #14856, #10346, #6667, #6550, #15133, #3929 ) ) ;
#15452 = DIRECTION ( 'NONE',  ( 0.5000000000000046629, -0.8660254037844359321, -6.938893903907214573E-16 ) ) ;
#15453 = CARTESIAN_POINT ( 'NONE',  ( 203.9371734008334158, 8.505830985348726614, -1.717498466822810599 ) ) ;
#15454 = DIRECTION ( 'NONE',  ( 0.000000000000000000, 0.000000000000000000, 1.000000000000000000 ) ) ;
#15455 = VECTOR ( 'NONE', #633, 1000.000000000000114 ) ;
#15456 = EDGE_CURVE ( 'NONE', #17966, #10122, #8250, .T. ) ;
#15458 = ORIENTED_EDGE ( 'NONE', *, *, #2941, .T. ) ;
#15457 = VERTEX_POINT ( 'NONE', #19490 ) ;
#15459 = ORIENTED_EDGE ( 'NONE', *, *, #20416, .F. ) ;
#15460 = VECTOR ( 'NONE', #19110, 1000.000000000000000 ) ;
#15461 = DIRECTION ( 'NONE',  ( -0.5000000000000049960, 0.8660254037844357100, -0.000000000000000000 ) ) ;
#15462 = CARTESIAN_POINT ( 'NONE',  ( 220.6020034895022945, 34.75287908616212462, -10.17395310825082433 ) ) ;
#15463 = EDGE_LOOP ( 'NONE', ( #5269, #9291, #8390, #14575 ) ) ;
#15464 = CARTESIAN_POINT ( 'NONE',  ( 210.6089461623840009, 5.465822580604545955, -25.65046807331635748 ) ) ;
#15465 = LINE ( 'NONE', #13754, #19668 ) ;
#15466 = DIRECTION ( 'NONE',  ( 0.000000000000000000, 1.000000000000000000, -1.295896757998782163E-15 ) ) ;
#15467 = DIRECTION ( 'NONE',  ( 0.000000000000000000, 0.000000000000000000, -1.000000000000000000 ) ) ;
#15468 = EDGE_CURVE ( 'NONE', #14274, #2250, #11378, .T. ) ;
#15469 = CARTESIAN_POINT ( 'NONE',  ( 199.3642739955437833, 5.865666282727633352, -4.003039906353938804 ) ) ;
#15470 = AXIS2_PLACEMENT_3D ( 'NONE', #13313, #3861, #2179 ) ;
#15471 = CONICAL_SURFACE ( 'NONE', #894, 14.00000000000000178, 0.7853981633974509435 ) ;
#15472 = VECTOR ( 'NONE', #2323, 1000.000000000000227 ) ;
#15473 = LINE ( 'NONE', #15573, #10463 ) ;
#15474 = CARTESIAN_POINT ( 'NONE',  ( 214.9156946368443926, 7.952324971666334008, -4.494676796018850951 ) ) ;
#15475 = CARTESIAN_POINT ( 'NONE',  ( -15.63876350448106223, 49.50806937060298196, -12.50030949268231062 ) ) ;
#15476 = DIRECTION ( 'NONE',  ( 0.7235536692358650601, 0.4177439057064745165, 0.5495089780708014571 ) ) ;
#15477 = CARTESIAN_POINT ( 'NONE',  ( 52.00490953756739287, 203.8812238888322383, 11.00000000000001066 ) ) ;
#15478 = ADVANCED_FACE ( 'NONE', ( #11343 ), #3594, .F. ) ;
#15479 = DIRECTION ( 'NONE',  ( -1.000000000000000000, -0.000000000000000000, -0.000000000000000000 ) ) ;
#15481 = ORIENTED_EDGE ( 'NONE', *, *, #1391, .F. ) ;
#15480 = EDGE_LOOP ( 'NONE', ( #4327, #14465, #3018, #13811 ) ) ;
#15482 = CARTESIAN_POINT ( 'NONE',  ( 198.3288405652164670, -0.8512796009538451392, -9.718744748712973447 ) ) ;
#15483 = CARTESIAN_POINT ( 'NONE',  ( 30.00000000000000355, 0.000000000000000000, -28.99999999999999645 ) ) ;
#15484 = CARTESIAN_POINT ( 'NONE',  ( -33.99999999999997868, 65.00000000000000000, -12.50000000000000000 ) ) ;
#15485 = ORIENTED_EDGE ( 'NONE', *, *, #15924, .T. ) ;
#15486 = AXIS2_PLACEMENT_3D ( 'NONE', #16183, #3234, #11497 ) ;
#15487 = ORIENTED_EDGE ( 'NONE', *, *, #12504, .F. ) ;
#15488 = CARTESIAN_POINT ( 'NONE',  ( 227.1212915979693037, 40.35032020428622701, -17.81526153211078523 ) ) ;
#15489 = CARTESIAN_POINT ( 'NONE',  ( 0.7736121223987986184, 51.05006296119952225, -6.934240817527092204 ) ) ;
#15490 = DIRECTION ( 'NONE',  ( -0.6299240516454600591, -0.3636868207865312508, -0.6862416378687270502 ) ) ;
#15491 = EDGE_CURVE ( 'NONE', #8387, #12920, #16134, .T. ) ;
#15492 = ORIENTED_EDGE ( 'NONE', *, *, #4317, .F. ) ;
#15493 = ORIENTED_EDGE ( 'NONE', *, *, #3327, .T. ) ;
#15494 = EDGE_CURVE ( 'NONE', #9425, #14892, #11550, .T. ) ;
#15495 = DIRECTION ( 'NONE',  ( 0.000000000000000000, 0.000000000000000000, 1.000000000000000000 ) ) ;
#15496 =( BOUNDED_SURFACE ( )  B_SPLINE_SURFACE ( 3, 2, ( 
 ( #14264, #10956, #16155 ),
 ( #6172, #8063, #18911 ),
 ( #4384, #17320, #12662 ),
 ( #2803, #11060, #1420 ),
 ( #7869, #14370, #12875 ),
 ( #17856, #3119, #44 ),
 ( #20905, #16068, #1630 ),
 ( #9770, #6482, #13185 ),
 ( #8282, #14690, #6379 ),
 ( #19330, #6585, #13085 ),
 ( #20806, #1840, #19234 ),
 ( #19528, #7878, #5002 ),
 ( #14792, #8074, #17538 ),
 ( #9458, #12983, #1429 ),
 ( #4806, #14479, #14379 ),
 ( #17647, #6278, #12771 ),
 ( #4700, #14583, #11169 ),
 ( #17751, #9570, #3216 ),
 ( #14895, #563, #15104 ),
 ( #3836, #10287, #3944 ),
 ( #5524, #10076, #3624 ),
 ( #8817, #18473, #7011 ),
 ( #8392, #11797, #11693 ),
 ( #9966, #18371, #7225 ),
 ( #1944, #355, #11589 ),
 ( #19736, #5412, #18159 ),
 ( #16460, #15004, #16567 ),
 ( #15210, #13498, #19944 ),
 ( #2256, #2360, #11907 ),
 ( #16674, #461, #661 ),
 ( #12011, #6802, #10390 ),
 ( #13288, #16881, #15318 ),
 ( #774, #2049, #3726 ),
 ( #8501, #18058, #6905 ) ),
 .UNSPECIFIED., .F., .F., .T. ) 
 B_SPLINE_SURFACE_WITH_KNOTS ( ( 4, 2, 2, 2, 2, 2, 2, 2, 2, 2, 2, 2, 2, 2, 2, 2, 4 ),
 ( 3, 3 ),
 ( 0.01278509310405299623, 0.01434830319407979539, 0.01591151328410659455, 0.01669311832911999499, 0.01747472337413339197, 0.01903793346416018939, 0.02060114355418698681, 0.02216435364421378423, 0.02529077382426737908, 0.02685398391429417650, 0.02841719400432097392, 0.03154361418437456877, 0.03310682427440136966, 0.03467003436442817055, 0.03623324445445497144, 0.03701484949946837189, 0.03779645454448176539 ),
 ( 0.000000000000000000, 1.000000000000000000 ),
 .UNSPECIFIED. ) 
 GEOMETRIC_REPRESENTATION_ITEM ( )  RATIONAL_B_SPLINE_SURFACE ( (
 ( 1.000000000000000000, 0.7167790485004659207, 1.000000000000000000),
 ( 1.000000000000000000, 0.7293845257053636066, 1.000000000000000000),
 ( 1.000000000000000000, 0.7423068803281102079, 1.000000000000000000),
 ( 1.000000000000000000, 0.7686138469776572224, 1.000000000000000000),
 ( 1.000000000000000000, 0.7816781719490264457, 1.000000000000000000),
 ( 1.000000000000000000, 0.8009424076554686467, 1.000000000000000000),
 ( 1.000000000000000000, 0.8073105603345962500, 1.000000000000000000),
 ( 1.000000000000000000, 0.8199112611634222780, 1.000000000000000000),
 ( 1.000000000000000000, 0.8261570471472956534, 1.000000000000000000),
 ( 1.000000000000000000, 0.8443914605100442117, 1.000000000000000000),
 ( 1.000000000000000000, 0.8559617003901804910, 1.000000000000000000),
 ( 1.000000000000000000, 0.8778584927324852849, 1.000000000000000000),
 ( 1.000000000000000000, 0.8881844774554348287, 1.000000000000000000),
 ( 1.000000000000000000, 0.9075144288648713253, 1.000000000000000000),
 ( 1.000000000000000000, 0.9165151951640571060, 1.000000000000000000),
 ( 1.000000000000000000, 0.9409273377063475108, 1.000000000000000000),
 ( 1.000000000000000000, 0.9539926103734300833, 1.000000000000000000),
 ( 1.000000000000000000, 0.9694264545131714428, 1.000000000000000000),
 ( 1.000000000000000000, 0.9738877056527739384, 1.000000000000000000),
 ( 1.000000000000000000, 0.9815112523102276221, 1.000000000000000000),
 ( 1.000000000000000000, 0.9846522094487469845, 1.000000000000000000),
 ( 1.000000000000000000, 0.9924326897349095011, 1.000000000000000000),
 ( 1.000000000000000000, 0.9954310229819894884, 1.000000000000000000),
 ( 1.000000000000000000, 0.9981072485120531246, 1.000000000000000000),
 ( 1.000000000000000000, 0.9986952519232461523, 1.000000000000000000),
 ( 1.000000000000000000, 0.9994860253291804053, 1.000000000000000000),
 ( 1.000000000000000000, 0.9996937099786900038, 1.000000000000000000),
 ( 1.000000000000000000, 0.9999366964164366767, 1.000000000000000000),
 ( 1.000000000000000000, 0.9999724247964512092, 1.000000000000000000),
 ( 1.000000000000000000, 0.9999959980224297773, 1.000000000000000000),
 ( 1.000000000000000000, 0.9999982534776523657, 1.000000000000000000),
 ( 1.000000000000000000, 1.000000247701407607, 1.000000000000000000),
 ( 1.000000000000000000, 1.000000000000000000, 1.000000000000000000),
 ( 1.000000000000000000, 1.000000000000000000, 1.000000000000000000) ) ) 
 REPRESENTATION_ITEM ( '' )  SURFACE ( )  );
#15497 = DIRECTION ( 'NONE',  ( 0.8660254037844355990, 0.5000000000000054401, 0.000000000000000000 ) ) ;
#15498 = DIRECTION ( 'NONE',  ( 0.000000000000000000, 0.000000000000000000, -1.000000000000000000 ) ) ;
#15499 = EDGE_CURVE ( 'NONE', #5375, #13099, #13082, .T. ) ;
#15500 = CIRCLE ( 'NONE', #6319, 0.4000000000000001887 ) ;
#15501 = ORIENTED_EDGE ( 'NONE', *, *, #13807, .T. ) ;
#15502 = DIRECTION ( 'NONE',  ( -0.5000000000000045519, 0.8660254037844360431, 0.000000000000000000 ) ) ;
#15503 = CARTESIAN_POINT ( 'NONE',  ( 219.1096994420543922, 36.51014630340510081, -14.00000000000005507 ) ) ;
#15504 = AXIS2_PLACEMENT_3D ( 'NONE', #10030, #1800, #4 ) ;
#15505 = CARTESIAN_POINT ( 'NONE',  ( -15.99999999999999289, 5.000000000000000000, 0.000000000000000000 ) ) ;
#15506 = CARTESIAN_POINT ( 'NONE',  ( 215.8932031078481941, 9.031895989412584314, -5.050953241461466625 ) ) ;
#15507 = LINE ( 'NONE', #964, #14026 ) ;
#15508 = CARTESIAN_POINT ( 'NONE',  ( 219.8596994420544206, 35.21110819772841438, -14.00000000000005507 ) ) ;
#15509 = ORIENTED_EDGE ( 'NONE', *, *, #4882, .T. ) ;
#15511 = EDGE_CURVE ( 'NONE', #13175, #3796, #11767, .T. ) ;
#15510 = DIRECTION ( 'NONE',  ( 0.5000000000000045519, -0.8660254037844361541, -0.000000000000000000 ) ) ;
#15512 = VERTEX_POINT ( 'NONE', #16534 ) ;
#15513 = ORIENTED_EDGE ( 'NONE', *, *, #15580, .T. ) ;
#15514 = FACE_OUTER_BOUND ( 'NONE', #18282, .T. ) ;
#15515 = CARTESIAN_POINT ( 'NONE',  ( 34.99529059433362477, 263.3427481158986438, -28.99999999999998934 ) ) ;
#15516 = EDGE_CURVE ( 'NONE', #12209, #4965, #20163, .T. ) ;
#15517 = TOROIDAL_SURFACE ( 'NONE', #2985, 5.400000000000000355, 0.4000000000000000222 ) ;
#15518 = DIRECTION ( 'NONE',  ( 0.000000000000000000, 0.000000000000000000, -1.000000000000000000 ) ) ;
#15519 = CONICAL_SURFACE ( 'NONE', #13808, 1.499999999999990896, 1.503565061787116353 ) ;
#15520 = DIRECTION ( 'NONE',  ( 0.5171545105027488543, 0.2985792958513952544, -0.8021231927550450669 ) ) ;
#15521 = VERTEX_POINT ( 'NONE', #13782 ) ;
#15522 =( NAMED_UNIT ( * ) SI_UNIT ( $, .STERADIAN. ) SOLID_ANGLE_UNIT ( ) );
#15523 = ORIENTED_EDGE ( 'NONE', *, *, #14106, .T. ) ;
#15524 = CARTESIAN_POINT ( 'NONE',  ( 226.0313364130699370, 42.89117477760235886, -12.96012118015694448 ) ) ;
#15525 = CARTESIAN_POINT ( 'NONE',  ( 30.00000000000000000, 0.000000000000000000, 15.00000000000000000 ) ) ;
#15526 = DIRECTION ( 'NONE',  ( 0.8660254037844355990, 0.5000000000000054401, 0.000000000000000000 ) ) ;
#15527 = ADVANCED_FACE ( 'NONE', ( #7193 ), #740, .F. ) ;
#15528 = EDGE_CURVE ( 'NONE', #6296, #17439, #16744, .T. ) ;
#15529 = CARTESIAN_POINT ( 'NONE',  ( 62.00490953756744972, 186.5607158131434744, 26.00000000000001776 ) ) ;
#15530 = CARTESIAN_POINT ( 'NONE',  ( 210.7044991792821236, 12.94399760702244073, -24.25943249057096907 ) ) ;
#15531 = CIRCLE ( 'NONE', #16535, 4.999999999999976907 ) ;
#15532 = DIRECTION ( 'NONE',  ( 0.000000000000000000, 0.7559289460184550613, -0.6546536707079765316 ) ) ;
#15533 = PRODUCT_DEFINITION_SHAPE ( 'NONE', 'NONE',  #19104 ) ;
#15534 = ORIENTED_EDGE ( 'NONE', *, *, #1872, .T. ) ;
#15536 = EDGE_CURVE ( 'NONE', #14507, #17368, #10466, .T. ) ;
#15535 = SURFACE_SIDE_STYLE ('',( #20380 ) ) ;
#15537 = CARTESIAN_POINT ( 'NONE',  ( -3.544689826710143432, 78.99734867018932505, 1.332611642696186927 ) ) ;
#15538 = PLANE ( 'NONE',  #7846 ) ;
#15539 = LINE ( 'NONE', #12452, #18229 ) ;
#15541 = VERTEX_POINT ( 'NONE', #5487 ) ;
#15540 = ORIENTED_EDGE ( 'NONE', *, *, #15118, .F. ) ;
#15542 = ORIENTED_EDGE ( 'NONE', *, *, #5843, .F. ) ;
#15543 = ORIENTED_EDGE ( 'NONE', *, *, #11499, .T. ) ;
#15544 = CARTESIAN_POINT ( 'NONE',  ( -15.34250122215976653, 10.13184782583976684, 12.48692088216763985 ) ) ;
#15545 = SURFACE_STYLE_FILL_AREA ( #20179 ) ;
#15546 = ORIENTED_EDGE ( 'NONE', *, *, #16792, .F. ) ;
#15547 = PRODUCT_DEFINITION_CONTEXT ( 'detailed design', #14501, 'design' ) ;
#15548 = ADVANCED_FACE ( 'NONE', ( #7089 ), #5379, .T. ) ;
#15549 = DIRECTION ( 'NONE',  ( -0.8660254037844380415, -0.5000000000000014433, -0.000000000000000000 ) ) ;
#15550 = CARTESIAN_POINT ( 'NONE',  ( 46.88067919638974956, 212.7566511894377754, 48.96815749462641065 ) ) ;
#15551 = DIRECTION ( 'NONE',  ( 0.000000000000000000, 0.9841898184435619035, -0.1771169141330907193 ) ) ;
#15552 = LINE ( 'NONE', #2500, #764 ) ;
#15553 = B_SPLINE_CURVE_WITH_KNOTS ( 'NONE', 3,
 ( #6728, #1671, #89, #18198 ),
 .UNSPECIFIED., .F., .F.,
 ( 4, 4 ),
 ( 3.426792995114292227E-07, 0.0008543284172819957511 ),
 .UNSPECIFIED. ) ;
#15554 = DIRECTION ( 'NONE',  ( 0.000000000000000000, 0.000000000000000000, 1.000000000000000000 ) ) ;
#15555 = ORIENTED_EDGE ( 'NONE', *, *, #369, .T. ) ;
#15556 = CARTESIAN_POINT ( 'NONE',  ( 226.3972337354671538, 42.58389110082306672, -15.84136033874741756 ) ) ;
#15557 = DIRECTION ( 'NONE',  ( -0.8660254037844357100, -0.5000000000000051070, 0.000000000000000000 ) ) ;
#15558 = CARTESIAN_POINT ( 'NONE',  ( 228.0438635544405486, 39.07888546060046764, -10.26496874235367507 ) ) ;
#15559 = CARTESIAN_POINT ( 'NONE',  ( 24.01452848080067071, 222.3619860023652564, 26.00000000000001776 ) ) ;
#15560 = CARTESIAN_POINT ( 'NONE',  ( 201.5350480436278531, 7.118963263738831593, -2.551678190571418092 ) ) ;
#15561 = VECTOR ( 'NONE', #14327, 1000.000000000000000 ) ;
#15562 = ORIENTED_EDGE ( 'NONE', *, *, #19625, .T. ) ;
#15563 = ORIENTED_EDGE ( 'NONE', *, *, #13405, .T. ) ;
#15564 = CYLINDRICAL_SURFACE ( 'NONE', #12234, 12.47473710546057646 ) ;
#15565 = ORIENTED_EDGE ( 'NONE', *, *, #3319, .F. ) ;
#15566 = VERTEX_POINT ( 'NONE', #2332 ) ;
#15567 = CARTESIAN_POINT ( 'NONE',  ( -20.74074359463745765, 13.47737252516389184, 11.56691115307346251 ) ) ;
#15568 = CARTESIAN_POINT ( 'NONE',  ( 196.8077463644258387, 4.389654366710942668, -7.132002368301173512 ) ) ;
#15569 = CARTESIAN_POINT ( 'NONE',  ( 221.8919835788506987, 32.51856803065840040, -16.00491213559322290 ) ) ;
#15570 = FACE_OUTER_BOUND ( 'NONE', #18780, .T. ) ;
#15571 = SURFACE_STYLE_FILL_AREA ( #14398 ) ;
#15572 = ORIENTED_EDGE ( 'NONE', *, *, #10054, .F. ) ;
#15573 = CARTESIAN_POINT ( 'NONE',  ( 32.36389338619004263, 157.9004617752989930, -29.00000000000000000 ) ) ;
#15574 = CARTESIAN_POINT ( 'NONE',  ( 213.8895336909654361, 8.132690763974602888, -24.79563718815146345 ) ) ;
#15575 = CARTESIAN_POINT ( 'NONE',  ( -23.33357341442864197, 49.70767121013135892, -10.13114767712223951 ) ) ;
#15576 = CARTESIAN_POINT ( 'NONE',  ( 228.3653048450253209, 39.17509194615954726, -17.81526153211079588 ) ) ;
#15577 = AXIS2_PLACEMENT_3D ( 'NONE', #7363, #20894, #9446 ) ;
#15578 = CARTESIAN_POINT ( 'NONE',  ( 227.9553588074475954, 39.88513931160571957, -14.00000000000005507 ) ) ;
#15579 = DIRECTION ( 'NONE',  ( -0.4999999999999995004, 0.8660254037844390407, 0.000000000000000000 ) ) ;
#15580 = EDGE_CURVE ( 'NONE', #4012, #14976, #20228, .T. ) ;
#15582 = ORIENTED_EDGE ( 'NONE', *, *, #14494, .T. ) ;
#15581 = VERTEX_POINT ( 'NONE', #12304 ) ;
#15583 = CARTESIAN_POINT ( 'NONE',  ( 203.1748324726931401, 24.07643182039328877, -13.24616221489253576 ) ) ;
#15584 = CARTESIAN_POINT ( 'NONE',  ( 208.9119903699346708, 11.37804290162847209, -2.044871543907030631 ) ) ;
#15585 = DIRECTION ( 'NONE',  ( 0.5000000000000051070, -0.8660254037844355990, -1.942890293094023946E-16 ) ) ;
#15586 = ORIENTED_EDGE ( 'NONE', *, *, #12651, .F. ) ;
#15587 = LINE ( 'NONE', #7611, #19674 ) ;
#15588 = FACE_OUTER_BOUND ( 'NONE', #20573, .T. ) ;
#15589 = CARTESIAN_POINT ( 'NONE',  ( -31.27810441140633202, 50.29222651548906953, -9.535589147757439932 ) ) ;
#15590 = CARTESIAN_POINT ( 'NONE',  ( 44.00000000000000000, -10.00000000000000000, -15.00000000000000355 ) ) ;
#15591 = ORIENTED_EDGE ( 'NONE', *, *, #6732, .F. ) ;
#15592 = ORIENTED_EDGE ( 'NONE', *, *, #9617, .T. ) ;
#15593 = DIRECTION ( 'NONE',  ( -1.000000000000000000, -0.000000000000000000, -0.000000000000000000 ) ) ;
#15594 = ORIENTED_EDGE ( 'NONE', *, *, #4367, .T. ) ;
#15595 = LINE ( 'NONE', #6123, #14169 ) ;
#15596 = DIRECTION ( 'NONE',  ( 0.000000000000000000, -1.000000000000000000, 0.000000000000000000 ) ) ;
#15597 = DIRECTION ( 'NONE',  ( 0.6634139481689350637, 0.3830222215594922264, -0.6427876096865409172 ) ) ;
#15598 = CARTESIAN_POINT ( 'NONE',  ( 228.8726778135066127, 37.31683029529983742, -16.83383072344321008 ) ) ;
#15599 = DIRECTION ( 'NONE',  ( -0.8601696498176553130, -0.4966191788709760080, 0.1160929141252378949 ) ) ;
#15600 = CYLINDRICAL_SURFACE ( 'NONE', #16015, 5.999999999999998224 ) ;
#15601 = AXIS2_PLACEMENT_3D ( 'NONE', #3002, #7866, #20793 ) ;
#15602 = ADVANCED_FACE ( 'NONE', ( #5589 ), #6979, .T. ) ;
#15603 = DIRECTION ( 'NONE',  ( 0.8660254037844368202, 0.5000000000000031086, -1.942890293094023946E-16 ) ) ;
#15604 = AXIS2_PLACEMENT_3D ( 'NONE', #20171, #7129, #14904 ) ;
#15605 = FACE_BOUND ( 'NONE', #9601, .T. ) ;
#15606 = LINE ( 'NONE', #2562, #20046 ) ;
#15607 = EDGE_CURVE ( 'NONE', #1224, #10243, #842, .T. ) ;
#15608 = ORIENTED_EDGE ( 'NONE', *, *, #11119, .T. ) ;
#15609 = CARTESIAN_POINT ( 'NONE',  ( 79.56209656442725020, 66.33713882184865440, 0.4323996719432884883 ) ) ;
#15610 = CIRCLE ( 'NONE', #18988, 12.47473710546057823 ) ;
#15611 = VERTEX_POINT ( 'NONE', #18548 ) ;
#15612 = ORIENTED_EDGE ( 'NONE', *, *, #15899, .T. ) ;
#15613 = VERTEX_POINT ( 'NONE', #12184 ) ;
#15614 = CARTESIAN_POINT ( 'NONE',  ( -4.498188040268487953, 64.25000000000001421, 4.917720511238719894 ) ) ;
#15615 = CARTESIAN_POINT ( 'NONE',  ( 80.82197242644828350, 53.59722411448979074, -3.626216797365716005 ) ) ;
#15616 = VECTOR ( 'NONE', #3508, 1000.000000000000114 ) ;
#15617 =( BOUNDED_CURVE ( )  B_SPLINE_CURVE ( 3, ( #9461, #20909, #1434, #17957 ),
 .UNSPECIFIED., .F., .T. ) 
 B_SPLINE_CURVE_WITH_KNOTS ( ( 4, 4 ),
 ( 4.712388980384689674, 6.283185307179586232 ),
 .UNSPECIFIED. ) 
 CURVE ( )  GEOMETRIC_REPRESENTATION_ITEM ( )  RATIONAL_B_SPLINE_CURVE ( ( 1.000000000000000000, 0.8047378541243649375, 0.8047378541243649375, 1.000000000000000000 ) ) 
 REPRESENTATION_ITEM ( '' )  );
#15618 = EDGE_CURVE ( 'NONE', #15277, #5032, #18802, .T. ) ;
#15619 = DIRECTION ( 'NONE',  ( 0.000000000000000000, 0.000000000000000000, 1.000000000000000000 ) ) ;
#15620 = CIRCLE ( 'NONE', #5756, 12.47473710546057823 ) ;
#15621 = AXIS2_PLACEMENT_3D ( 'NONE', #5771, #7262, #19880 ) ;
#15622 = DIRECTION ( 'NONE',  ( 0.000000000000000000, 0.000000000000000000, -1.000000000000000000 ) ) ;
#15623 = VERTEX_POINT ( 'NONE', #15180 ) ;
#15624 = LINE ( 'NONE', #20678, #14183 ) ;
#15625 = CARTESIAN_POINT ( 'NONE',  ( 191.5478494775925640, 36.18576207517880050, -14.00000000000006395 ) ) ;
#15626 = CARTESIAN_POINT ( 'NONE',  ( 227.9553588074475670, 39.88513931160575510, -14.00000000000005507 ) ) ;
#15627 = LINE ( 'NONE', #18791, #17297 ) ;
#15628 = EDGE_CURVE ( 'NONE', #423, #4969, #7293, .T. ) ;
#15629 = VECTOR ( 'NONE', #1329, 1000.000000000000227 ) ;
#15630 = CARTESIAN_POINT ( 'NONE',  ( 182.3972143829816446, 2.035126980567696364, -22.00000000000003908 ) ) ;
#15631 = ADVANCED_FACE ( 'NONE', ( #18760 ), #13571, .F. ) ;
#15632 = VECTOR ( 'NONE', #20578, 1000.000000000000227 ) ;
#15633 = DIRECTION ( 'NONE',  ( 0.8137976813493725814, 0.4698463103929604867, 0.3420201433256626622 ) ) ;
#15634 = FACE_OUTER_BOUND ( 'NONE', #9355, .T. ) ;
#15635 = CARTESIAN_POINT ( 'NONE',  ( 228.3868406476923667, 39.13779084175868661, -9.834987871251060554 ) ) ;
#15636 = ORIENTED_EDGE ( 'NONE', *, *, #8968, .T. ) ;
#15637 = AXIS2_PLACEMENT_3D ( 'NONE', #8164, #14676, #16444 ) ;
#15638 = DIRECTION ( 'NONE',  ( 0.000000000000000000, 0.000000000000000000, 1.000000000000000000 ) ) ;
#15639 = CARTESIAN_POINT ( 'NONE',  ( 200.9574494032262066, -0.1064716713780056168, -23.53124788243904320 ) ) ;
#15640 = FACE_OUTER_BOUND ( 'NONE', #16227, .T. ) ;
#15641 = CARTESIAN_POINT ( 'NONE',  ( -14.95727968274949404, 79.99998834348832588, -12.47960036978351894 ) ) ;
#15643 = ORIENTED_EDGE ( 'NONE', *, *, #19823, .T. ) ;
#15642 = ORIENTED_EDGE ( 'NONE', *, *, #169, .T. ) ;
#15644 = ADVANCED_FACE ( 'NONE', ( #16952 ), #4932, .T. ) ;
#15645 = DIRECTION ( 'NONE',  ( 0.5000000000000052180, -0.8660254037844355990, 2.220446049250312341E-16 ) ) ;
#15646 = FILL_AREA_STYLE_COLOUR ( '', #11570 ) ;
#15647 = EDGE_LOOP ( 'NONE', ( #778, #8568 ) ) ;
#15648 = VECTOR ( 'NONE', #20730, 1000.000000000000114 ) ;
#15649 = CARTESIAN_POINT ( 'NONE',  ( 221.5988438203954729, 32.40845261667698907, -12.62147488791611849 ) ) ;
#15650 = CARTESIAN_POINT ( 'NONE',  ( 10.40000000000000568, 0.000000000000000000, 0.000000000000000000 ) ) ;
#15651 = VECTOR ( 'NONE', #6823, 1000.000000000000114 ) ;
#15652 = CARTESIAN_POINT ( 'NONE',  ( -34.33334827330879335, 65.74999999999997158, 2.147472525011942857 ) ) ;
#15653 = EDGE_CURVE ( 'NONE', #2505, #16451, #4128, .T. ) ;
#15654 = VECTOR ( 'NONE', #16212, 1000.000000000000000 ) ;
#15655 = CARTESIAN_POINT ( 'NONE',  ( 174.9952905943348469, 20.85563505625644609, -19.00000000000000355 ) ) ;
#15656 = ORIENTED_EDGE ( 'NONE', *, *, #11564, .F. ) ;
#15657 = CARTESIAN_POINT ( 'NONE',  ( -34.00000000000000711, 65.00000000000000000, -12.50000000000000000 ) ) ;
#15658 = CARTESIAN_POINT ( 'NONE',  ( 215.4868200432858600, 15.17402258341379451, -8.415281845792092597 ) ) ;
#15659 = CARTESIAN_POINT ( 'NONE',  ( 191.1694443951678863, 35.60712985292571631, -19.00000000000003908 ) ) ;
#15660 = EDGE_CURVE ( 'NONE', #11812, #2307, #949, .T. ) ;
#15661 = CARTESIAN_POINT ( 'NONE',  ( 190.7433706042750146, 35.72129598111152404, -9.000000000000062172 ) ) ;
#15662 = CARTESIAN_POINT ( 'NONE',  ( 216.5944766886066759, 8.921570241161999704, -4.392917125964956426 ) ) ;
#15663 =( GEOMETRIC_REPRESENTATION_CONTEXT ( 3 ) GLOBAL_UNCERTAINTY_ASSIGNED_CONTEXT ( ( #17850 ) ) GLOBAL_UNIT_ASSIGNED_CONTEXT ( ( #19126, #6175, #19324 ) ) REPRESENTATION_CONTEXT ( 'NONE', 'WORKASPACE' ) );
#15664 = VERTEX_POINT ( 'NONE', #13884 ) ;
#15665 = VERTEX_POINT ( 'NONE', #20335 ) ;
#15666 = AXIS2_PLACEMENT_3D ( 'NONE', #17500, #2873, #12322 ) ;
#15667 = DIRECTION ( 'NONE',  ( 0.000000000000000000, -0.9982500481053682151, -0.05913409725048478921 ) ) ;
#15668 = CONICAL_SURFACE ( 'NONE', #18358, 13.07248899748297433, 0.6693469023067423196 ) ;
#15669 = EDGE_CURVE ( 'NONE', #5690, #10014, #19913, .T. ) ;
#15670 = AXIS2_PLACEMENT_3D ( 'NONE', #77, #12800, #18087 ) ;
#15671 = ORIENTED_EDGE ( 'NONE', *, *, #13801, .T. ) ;
#15672 = VERTEX_POINT ( 'NONE', #20849 ) ;
#15673 = PRODUCT_RELATED_PRODUCT_CATEGORY ( 'part', '', ( #15365 ) ) ;
#15674 = CARTESIAN_POINT ( 'NONE',  ( -19.05738717796882398, 11.12984937779420136, 12.12347222335699826 ) ) ;
#15675 = CARTESIAN_POINT ( 'NONE',  ( 225.8486002515921882, 43.53415216962802958, -14.58164069302991805 ) ) ;
#15676 = DIRECTION ( 'NONE',  ( 0.8660254037844372643, 0.5000000000000027756, -0.000000000000000000 ) ) ;
#15677 = EDGE_CURVE ( 'NONE', #4564, #4238, #7935, .T. ) ;
#15678 = CARTESIAN_POINT ( 'NONE',  ( 217.7559408036613604, 37.55104950179651979, -15.81459191843834944 ) ) ;
#15679 = CARTESIAN_POINT ( 'NONE',  ( 32.39721438298033007, 261.8427481158985302, -22.00000000000000355 ) ) ;
#15680 = VERTEX_POINT ( 'NONE', #15590 ) ;
#15681 = DIRECTION ( 'NONE',  ( -0.5000000000000049960, 0.8660254037844357100, -0.000000000000000000 ) ) ;
#15682 = AXIS2_PLACEMENT_3D ( 'NONE', #6359, #19308, #17732 ) ;
#15683 = CIRCLE ( 'NONE', #8150, 12.47473710546057823 ) ;
#15684 = CARTESIAN_POINT ( 'NONE',  ( 218.9607832949105273, 37.18362568106379484, -11.01522019104621464 ) ) ;
#15685 = CARTESIAN_POINT ( 'NONE',  ( -25.30425913992641185, 50.18878380057854116, -8.354022865946610921 ) ) ;
#15686 = DIRECTION ( 'NONE',  ( 0.5000000000000044409, -0.8660254037844360431, -4.006172263299080068E-16 ) ) ;
#15687 = AXIS2_PLACEMENT_3D ( 'NONE', #831, #8672, #15170 ) ;
#15688 = CARTESIAN_POINT ( 'NONE',  ( 200.1750369523376492, -0.5581977105158604235, -20.57673792763505460 ) ) ;
#15689 = LINE ( 'NONE', #20429, #3244 ) ;
#15691 = ORIENTED_EDGE ( 'NONE', *, *, #5947, .F. ) ;
#15690 = VERTEX_POINT ( 'NONE', #16009 ) ;
#15692 = DIRECTION ( 'NONE',  ( -0.06808332454812035528, 0.1179237772655450517, -0.9906859460363316439 ) ) ;
#15693 = CARTESIAN_POINT ( 'NONE',  ( 51.15554463217806358, 255.3523670591321206, -19.00000000000000711 ) ) ;
#15694 = CARTESIAN_POINT ( 'NONE',  ( -2.666657930126863363, 76.88745196853420794, -3.296735915517357451 ) ) ;
#15695 = VERTEX_POINT ( 'NONE', #1057 ) ;
#15696 = VERTEX_POINT ( 'NONE', #7819 ) ;
#15697 = LINE ( 'NONE', #12403, #9180 ) ;
#15698 = DIRECTION ( 'NONE',  ( 0.9537419254229455579, 0.000000000000000000, -0.3006265784832282684 ) ) ;
#15699 = CARTESIAN_POINT ( 'NONE',  ( -28.53155540363584208, 49.99238495923260928, -12.31184910487761996 ) ) ;
#15700 = CARTESIAN_POINT ( 'NONE',  ( -28.48501876579843639, 8.591569706101985560, -0.7004361938144425537 ) ) ;
#15701 = VECTOR ( 'NONE', #20628, 1000.000000000000227 ) ;
#15702 = ORIENTED_EDGE ( 'NONE', *, *, #10101, .T. ) ;
#15703 = ORIENTED_EDGE ( 'NONE', *, *, #9772, .T. ) ;
#15704 = DIRECTION ( 'NONE',  ( 0.000000000000000000, -1.000000000000000000, 0.000000000000000000 ) ) ;
#15705 = CARTESIAN_POINT ( 'NONE',  ( 208.8107687779841228, 4.427644383670616079, -14.00000000000005507 ) ) ;
#15706 = CARTESIAN_POINT ( 'NONE',  ( 10.40000000000000036, 0.000000000000000000, -5.400000000000001243 ) ) ;
#15707 = EDGE_CURVE ( 'NONE', #2559, #2640, #6275, .T. ) ;
#15708 = PRODUCT_DEFINITION_SHAPE ( 'NONE', 'NONE',  #8724 ) ;
#15709 = CARTESIAN_POINT ( 'NONE',  ( 205.8564897284660731, 2.721990579170014080, -25.44774858730788125 ) ) ;
#15710 = CARTESIAN_POINT ( 'NONE',  ( 66.19073749086841474, 149.3106491262846589, 41.00000000000001421 ) ) ;
#15711 = DIRECTION ( 'NONE',  ( 0.000000000000000000, 0.000000000000000000, 1.000000000000000000 ) ) ;
#15712 = DIRECTION ( 'NONE',  ( 0.000000000000000000, 1.302777330458572662E-15, 1.000000000000000000 ) ) ;
#15713 = LINE ( 'NONE', #12421, #789 ) ;
#15714 = VECTOR ( 'NONE', #12751, 1000.000000000000114 ) ;
#15715 = CARTESIAN_POINT ( 'NONE',  ( -27.42580490583086572, 69.03990363093173244, 5.071150534606303495 ) ) ;
#15716 = CARTESIAN_POINT ( 'NONE',  ( 221.3426408305072925, 31.33870282379080408, -12.85003623376113779 ) ) ;
#15717 = CARTESIAN_POINT ( 'NONE',  ( 226.5322088109231231, 42.02363833641166480, -16.68717795561658690 ) ) ;
#15718 = ORIENTED_EDGE ( 'NONE', *, *, #5009, .T. ) ;
#15719 = CARTESIAN_POINT ( 'NONE',  ( 74.25247827671769585, 71.10552778957739406, -0.9041564858560480200 ) ) ;
#15720 = ADVANCED_FACE ( 'NONE', ( #20643 ), #11115, .T. ) ;
#15721 = ORIENTED_EDGE ( 'NONE', *, *, #14306, .T. ) ;
#15722 = ORIENTED_EDGE ( 'NONE', *, *, #16146, .T. ) ;
#15723 = LINE ( 'NONE', #1185, #6774 ) ;
#15724 = LINE ( 'NONE', #1186, #211 ) ;
#15725 = SHAPE_DEFINITION_REPRESENTATION ( #13472, #16277 ) ;
#15726 = AXIS2_PLACEMENT_3D ( 'NONE', #2141, #544, #19928 ) ;
#15727 = ADVANCED_FACE ( 'NONE', ( #10788 ), #15799, .F. ) ;
#15728 = CARTESIAN_POINT ( 'NONE',  ( 203.0727098700125737, 1.114774528527234798, -25.36561010639676184 ) ) ;
#15729 = ORIENTED_EDGE ( 'NONE', *, *, #10228, .F. ) ;
#15730 = FILL_AREA_STYLE ('',( #12439 ) ) ;
#15731 = ADVANCED_FACE ( 'NONE', ( #7716 ), #15471, .T. ) ;
#15732 = FACE_OUTER_BOUND ( 'NONE', #12433, .T. ) ;
#15733 = DIRECTION ( 'NONE',  ( 0.000000000000000000, -1.000000000000000000, 0.000000000000000000 ) ) ;
#15734 = CARTESIAN_POINT ( 'NONE',  ( 206.4411508673863409, 9.951503049707822512, -1.545471579934816875 ) ) ;
#15735 = FACE_OUTER_BOUND ( 'NONE', #8167, .T. ) ;
#15736 = FACE_OUTER_BOUND ( 'NONE', #5811, .T. ) ;
#15737 = FACE_OUTER_BOUND ( 'NONE', #1910, .T. ) ;
#15738 = DIRECTION ( 'NONE',  ( 0.6958540455341998276, 0.000000000000000000, 0.7181832268395633712 ) ) ;
#15739 = ORIENTED_EDGE ( 'NONE', *, *, #3215, .F. ) ;
#15740 = CIRCLE ( 'NONE', #1846, 11.94520687646042667 ) ;
#15741 = FACE_OUTER_BOUND ( 'NONE', #14654, .T. ) ;
#15742 = DIRECTION ( 'NONE',  ( 0.5000000000000054401, -0.8660254037844354880, 0.000000000000000000 ) ) ;
#15743 = CARTESIAN_POINT ( 'NONE',  ( 5.000000000000004441, -2.342598717236899830, 4.057500000000059615 ) ) ;
#15745 = ORIENTED_EDGE ( 'NONE', *, *, #16516, .T. ) ;
#15744 = ORIENTED_EDGE ( 'NONE', *, *, #13957, .T. ) ;
#15746 = ORIENTED_EDGE ( 'NONE', *, *, #18030, .T. ) ;
#15747 = DIRECTION ( 'NONE',  ( 0.8660254037844355990, 0.5000000000000054401, 0.000000000000000000 ) ) ;
#15748 = DIRECTION ( 'NONE',  ( 0.000000000000000000, 1.000000000000000000, -1.355657144061424088E-15 ) ) ;
#15749 = EDGE_LOOP ( 'NONE', ( #14003, #6847, #17531, #9146, #8032 ) ) ;
#15750 = EDGE_CURVE ( 'NONE', #19333, #4182, #12407, .T. ) ;
#15751 = CARTESIAN_POINT ( 'NONE',  ( 67.79769812808454788, 78.36839442147740442, -22.50225811741774606 ) ) ;
#15752 = ORIENTED_EDGE ( 'NONE', *, *, #9229, .F. ) ;
#15753 = DIRECTION ( 'NONE',  ( 1.000000000000000000, 0.000000000000000000, 0.000000000000000000 ) ) ;
#15754 = EDGE_CURVE ( 'NONE', #2330, #4222, #6649, .T. ) ;
#15755 = CIRCLE ( 'NONE', #20464, 12.47473710546057823 ) ;
#15756 = PLANE ( 'NONE',  #7924 ) ;
#15757 = CARTESIAN_POINT ( 'NONE',  ( 201.5350480436278531, 7.118963263738831593, -2.551678190571418092 ) ) ;
#15758 = ADVANCED_FACE ( 'NONE', ( #10901 ), #4233, .F. ) ;
#15759 = ORIENTED_EDGE ( 'NONE', *, *, #17264, .T. ) ;
#15760 = DIRECTION ( 'NONE',  ( 1.000000000000000000, -0.000000000000000000, -0.000000000000000000 ) ) ;
#15761 = CARTESIAN_POINT ( 'NONE',  ( 218.1626406098745008, 38.35320191943676349, -14.00000000000005507 ) ) ;
#15762 = CARTESIAN_POINT ( 'NONE',  ( 203.8433579509713809, 8.805705967725675265, -25.96288910428599550 ) ) ;
#15763 = CARTESIAN_POINT ( 'NONE',  ( 98.91428619100422281, 200.0914894846855248, 11.00000000000001066 ) ) ;
#15764 = ORIENTED_EDGE ( 'NONE', *, *, #10423, .T. ) ;
#15765 = ORIENTED_EDGE ( 'NONE', *, *, #12462, .T. ) ;
#15766 = CARTESIAN_POINT ( 'NONE',  ( 7.999999999999998224, 0.000000000000000000, 0.000000000000000000 ) ) ;
#15767 = ADVANCED_FACE ( 'NONE', ( #14319 ), #1268, .T. ) ;
#15768 = ORIENTED_EDGE ( 'NONE', *, *, #7208, .F. ) ;
#15769 = CIRCLE ( 'NONE', #8631, 13.99999999999999822 ) ;
#15770 = CARTESIAN_POINT ( 'NONE',  ( 203.1960812450809897, 12.73300840892584063, -2.187257959407754804 ) ) ;
#15771 = CARTESIAN_POINT ( 'NONE',  ( 197.9607918626003311, -1.063772618484184918, -11.13829696442576811 ) ) ;
#15772 = CARTESIAN_POINT ( 'NONE',  ( -31.74999999999995737, 0.000000000000000000, 5.000000000000000888 ) ) ;
#15773 = EDGE_CURVE ( 'NONE', #20129, #18696, #6976, .T. ) ;
#15774 = CARTESIAN_POINT ( 'NONE',  ( 209.8909370991932519, 2.556737970610027499, -14.00000000000005507 ) ) ;
#15775 = DIRECTION ( 'NONE',  ( -1.000000000000000000, 0.000000000000000000, 0.000000000000000000 ) ) ;
#15776 = B_SPLINE_CURVE_WITH_KNOTS ( 'NONE', 3,
 ( #7686, #2626, #9171, #10652 ),
 .UNSPECIFIED., .F., .F.,
 ( 4, 4 ),
 ( 3.280426939632746066E-07, 0.0006729788347498066783 ),
 .UNSPECIFIED. ) ;
#15777 = ORIENTED_EDGE ( 'NONE', *, *, #15285, .F. ) ;
#15778 = FACE_OUTER_BOUND ( 'NONE', #15920, .T. ) ;
#15779 = ADVANCED_FACE ( 'NONE', ( #19572, #8228 ), #14636, .T. ) ;
#15780 = EDGE_CURVE ( 'NONE', #3348, #4596, #1128, .T. ) ;
#15781 = DIRECTION ( 'NONE',  ( 0.7559289460184535070, 0.000000000000000000, -0.6546536707079781969 ) ) ;
#15782 = CARTESIAN_POINT ( 'NONE',  ( -8.667048942563669200, 49.69984668619762402, -10.14481273401418449 ) ) ;
#15783 = CARTESIAN_POINT ( 'NONE',  ( 198.8278877809574965, -0.5631545566074300790, -19.61257667712936126 ) ) ;
#15784 = AXIS2_PLACEMENT_3D ( 'NONE', #1610, #12748, #8052 ) ;
#15785 = DIRECTION ( 'NONE',  ( 0.8660254037844372643, 0.5000000000000027756, -0.000000000000000000 ) ) ;
#15786 = CARTESIAN_POINT ( 'NONE',  ( 218.2668715373649775, 38.79744626964149035, -13.97349461567471174 ) ) ;
#15788 = VERTEX_POINT ( 'NONE', #5049 ) ;
#15787 = VERTEX_POINT ( 'NONE', #190 ) ;
#15789 = DIRECTION ( 'NONE',  ( 0.000000000000000000, 0.000000000000000000, 1.000000000000000000 ) ) ;
#15790 = FACE_OUTER_BOUND ( 'NONE', #1184, .T. ) ;
#15791 = ADVANCED_FACE ( 'NONE', ( #17904 ), #12925, .T. ) ;
#15792 = CARTESIAN_POINT ( 'NONE',  ( 197.7058429191240521, 9.563217833519331634, -4.494676796018654663 ) ) ;
#15793 = ORIENTED_EDGE ( 'NONE', *, *, #16233, .F. ) ;
#15794 = EDGE_LOOP ( 'NONE', ( #1435, #13357, #1392, #12981 ) ) ;
#15795 = DIRECTION ( 'NONE',  ( 0.4439426092011903302, -0.7689311547811512604, -0.4600650377311499839 ) ) ;
#15796 = DIRECTION ( 'NONE',  ( -1.000000000000000000, 0.000000000000000000, 5.175391130484829193E-17 ) ) ;
#15797 = CARTESIAN_POINT ( 'NONE',  ( -30.29050950868652237, 50.09228121850021154, -10.73328253952971778 ) ) ;
#15798 = CONICAL_SURFACE ( 'NONE', #14104, 10.85470691220533190, 0.8171114040043576665 ) ;
#15799 = PLANE ( 'NONE',  #4283 ) ;
#15800 = ORIENTED_EDGE ( 'NONE', *, *, #6546, .F. ) ;
#15801 = ORIENTED_EDGE ( 'NONE', *, *, #10025, .F. ) ;
#15802 = CIRCLE ( 'NONE', #7647, 7.960520131757807150 ) ;
#15803 = DIRECTION ( 'NONE',  ( 0.8660254037844372643, 0.5000000000000027756, -0.000000000000000000 ) ) ;
#15804 = CIRCLE ( 'NONE', #6619, 4.999999999999977796 ) ;
#15805 = EDGE_CURVE ( 'NONE', #12331, #20124, #11476, .T. ) ;
#15806 =( LENGTH_UNIT ( ) NAMED_UNIT ( * ) SI_UNIT ( .MILLI., .METRE. ) );
#15807 = CARTESIAN_POINT ( 'NONE',  ( 208.4761278624580711, 5.007259451653140125, -14.00000000000005507 ) ) ;
#15808 = CARTESIAN_POINT ( 'NONE',  ( 221.1877743307729531, 33.12044585814464881, -16.57782486433075775 ) ) ;
#15809 = CARTESIAN_POINT ( 'NONE',  ( 219.0819991370609330, 37.38560385231634342, -10.82724490084729929 ) ) ;
#15810 = CARTESIAN_POINT ( 'NONE',  ( 218.4949601902774248, 36.27103037639907512, -10.80501622924627902 ) ) ;
#15811 = CARTESIAN_POINT ( 'NONE',  ( 78.09128061238048701, 67.27484481498704838, -25.30919057591654209 ) ) ;
#15812 = CIRCLE ( 'NONE', #17143, 12.47473710546057823 ) ;
#15813 = DIRECTION ( 'NONE',  ( 0.5000000000000054401, -0.8660254037844354880, 0.000000000000000000 ) ) ;
#15814 = CARTESIAN_POINT ( 'NONE',  ( 219.3085917042504036, 36.99313401332681650, -17.45257705044830487 ) ) ;
#15815 = PLANE ( 'NONE',  #5813 ) ;
#15816 = CIRCLE ( 'NONE', #9347, 3.619616396367202782 ) ;
#15817 = EDGE_LOOP ( 'NONE', ( #18338, #19023, #15509, #17552 ) ) ;
#15818 = CARTESIAN_POINT ( 'NONE',  ( 80.06760114659269334, 65.96496744433481751, 0.4654826109615978758 ) ) ;
#15819 = ORIENTED_EDGE ( 'NONE', *, *, #15773, .T. ) ;
#15820 = ORIENTED_EDGE ( 'NONE', *, *, #1142, .F. ) ;
#15821 = PLANE ( 'NONE',  #4419 ) ;
#15822 = CARTESIAN_POINT ( 'NONE',  ( 216.7433590455158878, 9.780347600644502037, -22.03054070023868860 ) ) ;
#15823 = DIRECTION ( 'NONE',  ( 0.8660254037844370423, 0.5000000000000026645, -0.000000000000000000 ) ) ;
#15824 = VERTEX_POINT ( 'NONE', #17694 ) ;
#15825 = AXIS2_PLACEMENT_3D ( 'NONE', #9890, #9584, #6396 ) ;
#15826 = LINE ( 'NONE', #12333, #15214 ) ;
#15827 = CARTESIAN_POINT ( 'NONE',  ( 211.3681101147246011, 27.51407081612045857, -14.64810036304597496 ) ) ;
#15828 = DIRECTION ( 'NONE',  ( -0.8660254037844360431, -0.5000000000000044409, 5.976026924694052093E-17 ) ) ;
#15829 = CARTESIAN_POINT ( 'NONE',  ( 59.70164726310041203, 84.63482219402854412, -16.31058207722989195 ) ) ;
#15830 = PLANE ( 'NONE',  #15352 ) ;
#15831 = CARTESIAN_POINT ( 'NONE',  ( 208.2794616557154370, 15.66789945739891898, -26.10173121575784450 ) ) ;
#15832 = CARTESIAN_POINT ( 'NONE',  ( 194.1738290307969805, 7.524008664312185957, -9.972943347741734854 ) ) ;
#15833 = CARTESIAN_POINT ( 'NONE',  ( 51.15554463217806358, 255.3523670591321206, -13.99999999999994671 ) ) ;
#15834 = ORIENTED_EDGE ( 'NONE', *, *, #18715, .F. ) ;
#15835 = DIRECTION ( 'NONE',  ( 0.8660254037844370423, 0.5000000000000026645, -0.000000000000000000 ) ) ;
#15836 = CARTESIAN_POINT ( 'NONE',  ( 208.4761278624580711, 5.007259451653140125, -14.00000000000005507 ) ) ;
#15837 = CIRCLE ( 'NONE', #1605, 12.50000000000000000 ) ;
#15838 = EDGE_CURVE ( 'NONE', #1208, #1744, #18005, .T. ) ;
#15839 = CARTESIAN_POINT ( 'NONE',  ( 45.00000000000000000, 5.000000000000000000, 0.000000000000000000 ) ) ;
#15840 = CARTESIAN_POINT ( 'NONE',  ( 86.00000000000000000, 65.00000000000000000, -12.50000000000000000 ) ) ;
#15841 = CARTESIAN_POINT ( 'NONE',  ( -20.90625477759164141, 14.43164562092441372, 0.9643584936165373600 ) ) ;
#15842 = VECTOR ( 'NONE', #4708, 1000.000000000000000 ) ;
#15844 = VERTEX_POINT ( 'NONE', #16205 ) ;
#15843 = EDGE_LOOP ( 'NONE', ( #2204, #8465, #5018, #13527 ) ) ;
#15845 = ORIENTED_EDGE ( 'NONE', *, *, #20711, .F. ) ;
#15846 = CARTESIAN_POINT ( 'NONE',  ( -11.16244655246401152, 13.79331584593744431, 11.52618815104203165 ) ) ;
#15847 = CARTESIAN_POINT ( 'NONE',  ( 191.7908974019474613, 16.76289617730678216, -23.06309126349794170 ) ) ;
#15848 = DIRECTION ( 'NONE',  ( 0.000000000000000000, 0.000000000000000000, -1.000000000000000000 ) ) ;
#15849 = CARTESIAN_POINT ( 'NONE',  ( 226.1456958721146577, 43.01956746017689426, -13.95414044509031548 ) ) ;
#15850 = EDGE_CURVE ( 'NONE', #2725, #13569, #224, .T. ) ;
#15851 = AXIS2_PLACEMENT_3D ( 'NONE', #9964, #11588, #11168 ) ;
#15852 = DIRECTION ( 'NONE',  ( 0.5000000000000044409, -0.8660254037844360431, -4.006172263299080068E-16 ) ) ;
#15853 = VECTOR ( 'NONE', #2654, 1000.000000000000227 ) ;
#15854 =( BOUNDED_CURVE ( )  B_SPLINE_CURVE ( 3, ( #3104, #20581, #6054, #14362 ),
 .UNSPECIFIED., .F., .F. ) 
 B_SPLINE_CURVE_WITH_KNOTS ( ( 4, 4 ),
 ( 4.712388980384689674, 4.899261154233307991 ),
 .UNSPECIFIED. ) 
 CURVE ( )  GEOMETRIC_REPRESENTATION_ITEM ( )  RATIONAL_B_SPLINE_CURVE ( ( 1.000000000000000000, 0.9970920157757060531, 0.9970920157757060531, 1.000000000000000000 ) ) 
 REPRESENTATION_ITEM ( '' )  );
#15855 = ORIENTED_EDGE ( 'NONE', *, *, #17940, .T. ) ;
#15856 = DIRECTION ( 'NONE',  ( 0.2483788854152947367, 0.1434016163555419388, -0.9579895123154918979 ) ) ;
#15857 = PLANE ( 'NONE',  #19891 ) ;
#15858 = CARTESIAN_POINT ( 'NONE',  ( 221.3208164193364951, 32.89001020120745267, -16.29291827778590118 ) ) ;
#15859 = EDGE_CURVE ( 'NONE', #16512, #12634, #16312, .T. ) ;
#15860 = DIRECTION ( 'NONE',  ( -0.5000000000000043299, 0.8660254037844361541, 1.272130549049658454E-16 ) ) ;
#15861 = EDGE_CURVE ( 'NONE', #18586, #2903, #13096, .T. ) ;
#15862 = VERTEX_POINT ( 'NONE', #13126 ) ;
#15863 = CARTESIAN_POINT ( 'NONE',  ( 221.3323636658532507, 33.48785815289731005, -17.20332536629375753 ) ) ;
#15864 = EDGE_LOOP ( 'NONE', ( #6544, #14804, #11600, #20130 ) ) ;
#15865 = ORIENTED_EDGE ( 'NONE', *, *, #16600, .F. ) ;
#15866 = CIRCLE ( 'NONE', #17204, 1.500000000000000444 ) ;
#15867 = CARTESIAN_POINT ( 'NONE',  ( 58.37797649651341203, 276.8427481158987007, -26.99999999999999289 ) ) ;
#15868 = DIRECTION ( 'NONE',  ( 0.000000000000000000, 0.000000000000000000, -1.000000000000000000 ) ) ;
#15869 = LINE ( 'NONE', #2932, #20193 ) ;
#15870 = ADVANCED_FACE ( 'NONE', ( #1678 ), #20852, .F. ) ;
#15871 = DIRECTION ( 'NONE',  ( -0.7071067811865489050, 8.168906669016238096E-17, -0.7071067811865460184 ) ) ;
#15872 = CARTESIAN_POINT ( 'NONE',  ( 200.1915427753721417, 0.2241520214996718663, -5.993340328401664863 ) ) ;
#15873 = ORIENTED_EDGE ( 'NONE', *, *, #5629, .F. ) ;
#15874 = CARTESIAN_POINT ( 'NONE',  ( 219.9859744069469230, 35.17192153991415182, -10.43865930680574827 ) ) ;
#15875 = EDGE_CURVE ( 'NONE', #17471, #804, #19326, .T. ) ;
#15876 = VECTOR ( 'NONE', #4044, 999.9999999999998863 ) ;
#15877 = ORIENTED_EDGE ( 'NONE', *, *, #10268, .F. ) ;
#15878 = FILL_AREA_STYLE ('',( #10996 ) ) ;
#15879 = CARTESIAN_POINT ( 'NONE',  ( -10.08519122218491404, 49.57845857190523731, -11.02153694242965187 ) ) ;
#15880 = CARTESIAN_POINT ( 'NONE',  ( 205.0662616026534693, 10.91332106064940888, -14.00000000000005507 ) ) ;
#15881 = EDGE_CURVE ( 'NONE', #14889, #5590, #8340, .T. ) ;
#15882 = PRODUCT_DEFINITION_FORMATION_WITH_SPECIFIED_SOURCE ( 'ANY', '', #8552, .NOT_KNOWN. ) ;
#15883 = LINE ( 'NONE', #9492, #14251 ) ;
#15884 = LINE ( 'NONE', #12599, #20507 ) ;
#15885 = VERTEX_POINT ( 'NONE', #8865 ) ;
#15886 = B_SPLINE_CURVE_WITH_KNOTS ( 'NONE', 3,
 ( #5296, #19514, #11788, #16557, #3715, #13278, #18251, #10169, #14994, #8488, #16665, #6786, #17844, #5195, #8173, #6574, #2146, #13073, #8597, #1723, #9956, #16448 ),
 .UNSPECIFIED., .F., .F.,
 ( 4, 2, 2, 2, 2, 2, 2, 2, 2, 2, 4 ),
 ( 0.000000000000000000, 0.002138836336596501835, 0.003208254504894771618, 0.004277672673193041834, 0.004812381757342193422, 0.005347090841491346745, 0.006416509009789626503, 0.006951218093938767682, 0.007485927178087907995, 0.008020636262237049174, 0.008555345346386189487 ),
 .UNSPECIFIED. ) ;
#15887 = VERTEX_POINT ( 'NONE', #4101 ) ;
#15888 = CARTESIAN_POINT ( 'NONE',  ( 201.7020968622623798, 0.3234507395478347092, -5.321846656828017608 ) ) ;
#15889 = DIRECTION ( 'NONE',  ( -0.1997192025788214753, -0.1153079353712215399, -0.9730448705798235842 ) ) ;
#15890 = CARTESIAN_POINT ( 'NONE',  ( -3.671937341326915849, 79.99999999995419842, -2.072940693968563064 ) ) ;
#15891 = ORIENTED_EDGE ( 'NONE', *, *, #15255, .F. ) ;
#15892 = ORIENTED_EDGE ( 'NONE', *, *, #5139, .F. ) ;
#15893 = DIRECTION ( 'NONE',  ( -0.000000000000000000, -1.000000000000000000, -0.000000000000000000 ) ) ;
#15894 = DIRECTION ( 'NONE',  ( 0.2961981327260295171, 0.1710100716628401019, 0.9396926207859056523 ) ) ;
#15895 = CARTESIAN_POINT ( 'NONE',  ( 1.475260119819425508, 52.70730118409597509, -3.895249003718037617 ) ) ;
#15896 = CARTESIAN_POINT ( 'NONE',  ( -25.99999999999999645, 9.999999999999994671, -7.500000000000000000 ) ) ;
#15897 = ORIENTED_EDGE ( 'NONE', *, *, #11536, .F. ) ;
#15898 = EDGE_CURVE ( 'NONE', #6007, #2199, #16828, .T. ) ;
#15899 = EDGE_CURVE ( 'NONE', #8072, #4749, #17501, .T. ) ;
#15900 = CIRCLE ( 'NONE', #8071, 5.000000000000005329 ) ;
#15901 = VERTEX_POINT ( 'NONE', #817 ) ;
#15902 = CARTESIAN_POINT ( 'NONE',  ( 229.4078764774343142, 37.36930490829751506, -17.10689588174069797 ) ) ;
#15903 = CARTESIAN_POINT ( 'NONE',  ( 0.000000000000000000, 0.000000000000000000, 0.000000000000000000 ) ) ;
#15904 = CARTESIAN_POINT ( 'NONE',  ( 225.8482621832700659, 43.53473772113840567, -13.42327856638894623 ) ) ;
#15905 = CARTESIAN_POINT ( 'NONE',  ( 209.3710013429994206, 26.91277392005484614, -18.25196083293883120 ) ) ;
#15906 = EDGE_CURVE ( 'NONE', #6947, #19116, #9009, .T. ) ;
#15907 = DIRECTION ( 'NONE',  ( 0.5000000000000054401, -0.8660254037844354880, -2.081668171172167774E-16 ) ) ;
#15908 = CARTESIAN_POINT ( 'NONE',  ( 199.1376418611926624, 24.40322754623966972, -14.00000000000005507 ) ) ;
#15909 = CARTESIAN_POINT ( 'NONE',  ( 202.0455819868764138, 0.5217619687064301015, -24.58554911381517627 ) ) ;
#15910 = B_SPLINE_CURVE_WITH_KNOTS ( 'NONE', 3,
 ( #2727, #5984, #9169, #17139 ),
 .UNSPECIFIED., .F., .F.,
 ( 4, 4 ),
 ( 4.145267926750471987E-07, 0.0005663407490910604778 ),
 .UNSPECIFIED. ) ;
#15911 = CARTESIAN_POINT ( 'NONE',  ( -31.81644051279125662, 65.48968590022897729, 2.492004793192827972 ) ) ;
#15912 = CARTESIAN_POINT ( 'NONE',  ( 228.8533067253947877, 37.35038200410757270, -11.12998660979008392 ) ) ;
#15913 = DIRECTION ( 'NONE',  ( -0.2597919750177127840, 0.4499729001293399921, -0.8544194045464951204 ) ) ;
#15914 = AXIS2_PLACEMENT_3D ( 'NONE', #20191, #7253, #10426 ) ;
#15915 = ORIENTED_EDGE ( 'NONE', *, *, #652, .F. ) ;
#15916 = AXIS2_PLACEMENT_3D ( 'NONE', #473, #13401, #12991 ) ;
#15917 = EDGE_CURVE ( 'NONE', #14739, #3127, #11725, .T. ) ;
#15918 = CARTESIAN_POINT ( 'NONE',  ( 69.70673644162950211, 71.32081881487549424, -1.123846180645351023 ) ) ;
#15919 = CIRCLE ( 'NONE', #12871, 4.999999999999995559 ) ;
#15920 = EDGE_LOOP ( 'NONE', ( #19328, #5427, #19046, #15591 ) ) ;
#15921 = VERTEX_POINT ( 'NONE', #13653 ) ;
#15922 = CARTESIAN_POINT ( 'NONE',  ( -3.132434197188862957, 70.94952981831174554, 1.317303739528327577 ) ) ;
#15923 = VECTOR ( 'NONE', #16872, 1000.000000000000000 ) ;
#15924 = EDGE_CURVE ( 'NONE', #9496, #4124, #13760, .T. ) ;
#15925 = CARTESIAN_POINT ( 'NONE',  ( 227.3709454187517451, 40.89737299345080146, -17.42570676230487337 ) ) ;
#15926 = PRODUCT_CONTEXT ( 'NONE', #2287, 'mechanical' ) ;
#15927 = CARTESIAN_POINT ( 'NONE',  ( 222.0128931678030710, 32.30914647947069795, -12.46964089162990952 ) ) ;
#15928 = ORIENTED_EDGE ( 'NONE', *, *, #12238, .T. ) ;
#15929 = DIRECTION ( 'NONE',  ( -0.000000000000000000, 1.000000000000000000, -0.000000000000000000 ) ) ;
#15930 = ORIENTED_EDGE ( 'NONE', *, *, #18722, .F. ) ;
#15931 = CONICAL_SURFACE ( 'NONE', #15263, 3.078786038154920579, 0.8168758188741392923 ) ;
#15932 = CARTESIAN_POINT ( 'NONE',  ( 209.9156946368443357, 16.61257900951069288, -4.494676796018852727 ) ) ;
#15933 = CARTESIAN_POINT ( 'NONE',  ( 226.6211368133091923, 39.11482588413117867, -14.00000000000005507 ) ) ;
#15934 = DIRECTION ( 'NONE',  ( -0.5000000000000057732, 0.8660254037844353769, 0.000000000000000000 ) ) ;
#15935 = VECTOR ( 'NONE', #4491, 1000.000000000000227 ) ;
#15936 = CARTESIAN_POINT ( 'NONE',  ( 99.99529059433426426, 150.7594456239217777, 21.00000000000000711 ) ) ;
#15937 = CARTESIAN_POINT ( 'NONE',  ( 203.7027818574982518, 1.478546760110915903, -24.25943249057081630 ) ) ;
#15938 = CARTESIAN_POINT ( 'NONE',  ( 226.1594288993896953, 42.99578115919451449, -13.55260094074449739 ) ) ;
#15939 = CARTESIAN_POINT ( 'NONE',  ( 229.6043086138720639, 37.02907446774801770, -16.68624095904344529 ) ) ;
#15940 = DIRECTION ( 'NONE',  ( -0.8660254037844360431, -0.5000000000000044409, 5.976026924694052093E-17 ) ) ;
#15941 = VERTEX_POINT ( 'NONE', #3996 ) ;
#15942 = CARTESIAN_POINT ( 'NONE',  ( 220.6096994420543922, 33.91207009205179901, -14.00000000000005507 ) ) ;
#15943 = VECTOR ( 'NONE', #5870, 1000.000000000000000 ) ;
#15944 = CARTESIAN_POINT ( 'NONE',  ( 58.80511404976427769, 85.32389451869947550, -10.75888619813460423 ) ) ;
#15945 = CARTESIAN_POINT ( 'NONE',  ( -15.99999999999999289, 65.74999999999998579, 4.999999999999989342 ) ) ;
#15946 = CIRCLE ( 'NONE', #2388, 3.902363844300875240 ) ;
#15947 = CARTESIAN_POINT ( 'NONE',  ( -15.99999999999999289, 0.000000000000000000, 0.000000000000000000 ) ) ;
#15948 = CARTESIAN_POINT ( 'NONE',  ( 0.000000000000000000, 4.685197434473814759, -6.938893903907228378E-15 ) ) ;
#15950 = VERTEX_POINT ( 'NONE', #16927 ) ;
#15949 = VERTEX_POINT ( 'NONE', #11744 ) ;
#15951 = VERTEX_POINT ( 'NONE', #16613 ) ;
#15952 = AXIS2_PLACEMENT_3D ( 'NONE', #4328, #14310, #17257 ) ;
#15953 = ORIENTED_EDGE ( 'NONE', *, *, #8314, .T. ) ;
#15954 = CARTESIAN_POINT ( 'NONE',  ( 209.9477407942357843, 12.50708294970442225, -14.41834690440041022 ) ) ;
#15955 = VECTOR ( 'NONE', #19071, 1000.000000000000227 ) ;
#15956 = B_SPLINE_CURVE_WITH_KNOTS ( 'NONE', 3,
 ( #3421, #16256, #17752, #13187 ),
 .UNSPECIFIED., .F., .F.,
 ( 4, 4 ),
 ( 3.531115201596283599E-07, 0.0004524063533000397550 ),
 .UNSPECIFIED. ) ;
#15957 = DIRECTION ( 'NONE',  ( 0.000000000000000000, 0.000000000000000000, 1.000000000000000000 ) ) ;
#15958 = VERTEX_POINT ( 'NONE', #2409 ) ;
#15959 = DIRECTION ( 'NONE',  ( 0.5000000000000041078, -0.8660254037844363761, 0.000000000000000000 ) ) ;
#15960 = AXIS2_PLACEMENT_3D ( 'NONE', #3979, #6934, #2392 ) ;
#15961 = AXIS2_PLACEMENT_3D ( 'NONE', #4521, #10651, #7478 ) ;
#15962 = EDGE_CURVE ( 'NONE', #4281, #279, #8965, .T. ) ;
#15963 = DIRECTION ( 'NONE',  ( -0.6518835024542932732, 0.000000000000000000, -0.7583191275630091210 ) ) ;
#15964 = CIRCLE ( 'NONE', #9840, 11.98469917212512215 ) ;
#15965 = VECTOR ( 'NONE', #7911, 1000.000000000000227 ) ;
#15966 = CIRCLE ( 'NONE', #16629, 3.619616396367202782 ) ;
#15967 = ORIENTED_EDGE ( 'NONE', *, *, #1207, .F. ) ;
#15968 = CARTESIAN_POINT ( 'NONE',  ( 218.9878548032870071, 10.30338773994525425, -15.39542905462748479 ) ) ;
#15969 = CARTESIAN_POINT ( 'NONE',  ( 221.0845718809542007, 33.50511594550124528, -17.03266613944940033 ) ) ;
#15970 = CARTESIAN_POINT ( 'NONE',  ( 203.9035579930133792, 8.663445801030889015, -26.12540443289068293 ) ) ;
#15971 = CARTESIAN_POINT ( 'NONE',  ( 226.4161948415057282, 42.55104950179654111, -15.81459191843835654 ) ) ;
#15972 = ORIENTED_EDGE ( 'NONE', *, *, #16041, .T. ) ;
#15973 = PLANE ( 'NONE',  #7145 ) ;
#15974 = ADVANCED_FACE ( 'NONE', ( #3886 ), #6954, .F. ) ;
#15975 = VECTOR ( 'NONE', #6602, 1000.000000000000000 ) ;
#15976 = EDGE_LOOP ( 'NONE', ( #18652, #7608, #8910, #15308 ) ) ;
#15977 = ORIENTED_EDGE ( 'NONE', *, *, #14886, .F. ) ;
#15978 = CARTESIAN_POINT ( 'NONE',  ( 209.9044635914013668, 29.65591986667770641, -11.50010063814821315 ) ) ;
#15979 = CARTESIAN_POINT ( 'NONE',  ( 221.5594486299148400, 33.09453545750766779, -16.83383072344321718 ) ) ;
#15980 = B_SPLINE_CURVE_WITH_KNOTS ( 'NONE', 3,
 ( #11078, #17231, #2719, #13960 ),
 .UNSPECIFIED., .F., .F.,
 ( 4, 4 ),
 ( 1.578338979776156445E-06, 0.0006742291310223107702 ),
 .UNSPECIFIED. ) ;
#15981 = FACE_OUTER_BOUND ( 'NONE', #20199, .T. ) ;
#15982 = CIRCLE ( 'NONE', #398, 5.000000000000005329 ) ;
#15983 = AXIS2_PLACEMENT_3D ( 'NONE', #4617, #20724, #7888 ) ;
#15984 = DIRECTION ( 'NONE',  ( 0.8660254037844355990, 0.5000000000000054401, 0.000000000000000000 ) ) ;
#15985 = CARTESIAN_POINT ( 'NONE',  ( 28.00000000000001066, 64.25000000000000000, -1.525597966175989972 ) ) ;
#15986 = EDGE_CURVE ( 'NONE', #2041, #5298, #14803, .T. ) ;
#15987 = ORIENTED_EDGE ( 'NONE', *, *, #17019, .T. ) ;
#15988 = ADVANCED_FACE ( 'NONE', ( #19889 ), #8763, .F. ) ;
#15989 = DIRECTION ( 'NONE',  ( 0.5000000000000007772, -0.8660254037844381525, 0.000000000000000000 ) ) ;
#15990 = VECTOR ( 'NONE', #5744, 1000.000000000000000 ) ;
#15991 = FACE_OUTER_BOUND ( 'NONE', #5077, .T. ) ;
#15992 = CARTESIAN_POINT ( 'NONE',  ( -10.36407271659200369, 45.24472543703319616, -11.16260780707907685 ) ) ;
#15993 = FACE_BOUND ( 'NONE', #5600, .T. ) ;
#15994 = AXIS2_PLACEMENT_3D ( 'NONE', #2916, #20494, #18816 ) ;
#15995 = LINE ( 'NONE', #20833, #7767 ) ;
#15996 = AXIS2_PLACEMENT_3D ( 'NONE', #12419, #9519, #11123 ) ;
#15997 = LINE ( 'NONE', #7906, #13084 ) ;
#15999 = ORIENTED_EDGE ( 'NONE', *, *, #1612, .F. ) ;
#15998 = ORIENTED_EDGE ( 'NONE', *, *, #15165, .T. ) ;
#16000 = LINE ( 'NONE', #12811, #11197 ) ;
#16001 = DIRECTION ( 'NONE',  ( -0.5016613886297202063, 0.000000000000000000, 0.8650640734408641119 ) ) ;
#16002 = CARTESIAN_POINT ( 'NONE',  ( -4.047976277355980201, 79.14876326484314006, -7.307758369674530741 ) ) ;
#16003 = ORIENTED_EDGE ( 'NONE', *, *, #8125, .T. ) ;
#16004 = ORIENTED_EDGE ( 'NONE', *, *, #5514, .F. ) ;
#16005 = ORIENTED_EDGE ( 'NONE', *, *, #3457, .T. ) ;
#16006 = DIRECTION ( 'NONE',  ( 0.5000000000000044409, -0.8660254037844360431, -0.000000000000000000 ) ) ;
#16007 = CARTESIAN_POINT ( 'NONE',  ( 228.7840727999461308, 37.79680543915253566, -10.90800523708426795 ) ) ;
#16008 = CARTESIAN_POINT ( 'NONE',  ( -32.72864378893952875, 57.92794788011308782, 0.7338665021735866212 ) ) ;
#16009 = CARTESIAN_POINT ( 'NONE',  ( 228.6672469504414664, 37.67264698757139030, -10.82724490084735791 ) ) ;
#16010 = VERTEX_POINT ( 'NONE', #922 ) ;
#16011 = EDGE_CURVE ( 'NONE', #1466, #14739, #8554, .T. ) ;
#16012 = ORIENTED_EDGE ( 'NONE', *, *, #20356, .F. ) ;
#16013 = CARTESIAN_POINT ( 'NONE',  ( 1.078027122475627042, 73.66227117401368218, -0.2439945722892260527 ) ) ;
#16014 = AXIS2_PLACEMENT_3D ( 'NONE', #7017, #2477, #16784 ) ;
#16015 = AXIS2_PLACEMENT_3D ( 'NONE', #18562, #10802, #20350 ) ;
#16016 = EDGE_CURVE ( 'NONE', #9600, #10039, #10177, .T. ) ;
#16017 = COLOUR_RGB ( '',0.7921568627450980005, 0.8196078431372548767, 0.9333333333333333481 ) ;
#16018 = DIRECTION ( 'NONE',  ( 0.8137976813493681405, 0.4698463103929584328, -0.3420201433256762624 ) ) ;
#16019 = DIRECTION ( 'NONE',  ( 0.06808332454812728030, -0.1179237772655570421, -0.9906859460363297565 ) ) ;
#16020 = CARTESIAN_POINT ( 'NONE',  ( 221.5400775418029298, 33.12808716631536043, -11.12998660979008569 ) ) ;
#16021 = CARTESIAN_POINT ( 'NONE',  ( 80.40479875449686631, 65.68600401853653636, -25.48291287448371278 ) ) ;
#16022 = EDGE_CURVE ( 'NONE', #5656, #14733, #13338, .T. ) ;
#16023 = EDGE_LOOP ( 'NONE', ( #5404, #14415, #5837, #738 ) ) ;
#16024 = CARTESIAN_POINT ( 'NONE',  ( -27.57431306967301765, 71.02946758568791097, 4.727326826884577393 ) ) ;
#16025 = CYLINDRICAL_SURFACE ( 'NONE', #7235, 3.902363844300889451 ) ;
#16026 = ADVANCED_FACE ( 'NONE', ( #13442 ), #13755, .F. ) ;
#16027 = ORIENTED_EDGE ( 'NONE', *, *, #16252, .T. ) ;
#16028 = AXIS2_PLACEMENT_3D ( 'NONE', #7404, #4457, #10479 ) ;
#16029 = CARTESIAN_POINT ( 'NONE',  ( 81.45372947444067790, 64.43233774075389420, 0.4901336013121079804 ) ) ;
#16030 = VERTEX_POINT ( 'NONE', #611 ) ;
#16031 = ORIENTED_EDGE ( 'NONE', *, *, #18761, .F. ) ;
#16032 = CARTESIAN_POINT ( 'NONE',  ( -2.019385899523460370, 64.25000000000001421, 2.827122728375884186 ) ) ;
#16033 = DIRECTION ( 'NONE',  ( -0.1005394128318083391, -0.05804645706261228610, 0.9932383577419438003 ) ) ;
#16034 = EDGE_CURVE ( 'NONE', #7029, #14580, #19837, .T. ) ;
#16035 = CARTESIAN_POINT ( 'NONE',  ( -30.62802697534700869, 79.12678444398457600, -7.447389982869642822 ) ) ;
#16036 = SHAPE_DEFINITION_REPRESENTATION ( #15186, #20473 ) ;
#16037 = EDGE_CURVE ( 'NONE', #15664, #4012, #1579, .T. ) ;
#16038 = CARTESIAN_POINT ( 'NONE',  ( 229.4660061303077327, 36.28915550503100462, -13.49489896056993743 ) ) ;
#16039 = ORIENTED_EDGE ( 'NONE', *, *, #13779, .F. ) ;
#16040 = DIRECTION ( 'NONE',  ( -0.000000000000000000, 1.000000000000000000, -0.000000000000000000 ) ) ;
#16041 = EDGE_CURVE ( 'NONE', #16971, #16434, #1239, .T. ) ;
#16042 = DIRECTION ( 'NONE',  ( 1.000000000000000000, 0.000000000000000000, -0.000000000000000000 ) ) ;
#16043 = CARTESIAN_POINT ( 'NONE',  ( 209.2413142193426268, 30.98740296050068821, -15.88417608133634751 ) ) ;
#16044 = CARTESIAN_POINT ( 'NONE',  ( 215.7047814394237832, 8.407904449549567616, -14.00000000000005329 ) ) ;
#16045 = FACE_OUTER_BOUND ( 'NONE', #614, .T. ) ;
#16046 = CARTESIAN_POINT ( 'NONE',  ( 218.1629906666871648, 38.35469480878496285, -13.98365758669813985 ) ) ;
#16047 = ADVANCED_FACE ( 'NONE', ( #9475 ), #12276, .F. ) ;
#16048 = CARTESIAN_POINT ( 'NONE',  ( 4.000000000000000000, 2.639212418033078489, 1.523749999999995053 ) ) ;
#16049 = DIRECTION ( 'NONE',  ( -1.000000000000000000, 0.000000000000000000, 0.000000000000000000 ) ) ;
#16050 = CARTESIAN_POINT ( 'NONE',  ( 218.4514296286660624, 36.34642752079201955, -17.14987233279964229 ) ) ;
#16051 = ADVANCED_FACE ( 'NONE', ( #13864 ), #3942, .T. ) ;
#16052 = CARTESIAN_POINT ( 'NONE',  ( 202.6586965015780208, 8.121741361019813255, -25.63868392505618488 ) ) ;
#16053 = ORIENTED_EDGE ( 'NONE', *, *, #12635, .T. ) ;
#16054 = CARTESIAN_POINT ( 'NONE',  ( 212.8103755628029319, 7.252024676415511628, -2.709673684914666314 ) ) ;
#16055 = CARTESIAN_POINT ( 'NONE',  ( 77.50589888911159164, 70.51031857425567750, 0.1958985337333214449 ) ) ;
#16056 = CARTESIAN_POINT ( 'NONE',  ( 80.00000000000000000, 0.000000000000000000, 0.000000000000000000 ) ) ;
#16057 = CARTESIAN_POINT ( 'NONE',  ( -14.99999999999999645, 5.000000000000000000, 15.00000000000000000 ) ) ;
#16058 = ADVANCED_FACE ( 'NONE', ( #15981 ), #12426, .T. ) ;
#16060 = EDGE_LOOP ( 'NONE', ( #9048, #8686 ) ) ;
#16059 = VERTEX_POINT ( 'NONE', #6198 ) ;
#16061 = VERTEX_POINT ( 'NONE', #1028 ) ;
#16062 = LINE ( 'NONE', #20800, #13961 ) ;
#16063 = VERTEX_POINT ( 'NONE', #4205 ) ;
#16064 = DIRECTION ( 'NONE',  ( -0.7235536692358586208, -0.4177439057064700756, 0.5495089780708132254 ) ) ;
#16065 = ORIENTED_EDGE ( 'NONE', *, *, #11381, .F. ) ;
#16066 = CARTESIAN_POINT ( 'NONE',  ( 227.8189912981924010, 39.46837563363482104, -10.20315278194657083 ) ) ;
#16067 = EDGE_CURVE ( 'NONE', #7703, #8807, #15869, .T. ) ;
#16068 = CARTESIAN_POINT ( 'NONE',  ( -29.44791497984978790, 77.20859777394102252, -3.699063880715452779 ) ) ;
#16069 = CARTESIAN_POINT ( 'NONE',  ( 34.99529059433363898, 263.3427481158985302, -5.999999999999973355 ) ) ;
#16070 = DIRECTION ( 'NONE',  ( 0.8660254037844352659, 0.5000000000000056621, 0.000000000000000000 ) ) ;
#16071 = VECTOR ( 'NONE', #1759, 1000.000000000000000 ) ;
#16072 = LINE ( 'NONE', #14386, #3417 ) ;
#16073 = DIRECTION ( 'NONE',  ( -0.05035489893517527266, -0.02907241445524010384, -0.9983081582712679536 ) ) ;
#16074 = ORIENTED_EDGE ( 'NONE', *, *, #9970, .F. ) ;
#16075 = DIRECTION ( 'NONE',  ( -1.000000000000000000, 0.000000000000000000, 0.000000000000000000 ) ) ;
#16076 = CARTESIAN_POINT ( 'NONE',  ( 209.0220424616560422, 2.055081417730487470, -14.00000000000005507 ) ) ;
#16077 = ORIENTED_EDGE ( 'NONE', *, *, #11708, .T. ) ;
#16078 = LINE ( 'NONE', #6496, #11216 ) ;
#16079 = B_SPLINE_CURVE_WITH_KNOTS ( 'NONE', 3,
 ( #641, #3702, #2023, #10154 ),
 .UNSPECIFIED., .F., .F.,
 ( 4, 4 ),
 ( 4.351832737440840046E-07, 0.0005663614055718004621 ),
 .UNSPECIFIED. ) ;
#16080 = ORIENTED_EDGE ( 'NONE', *, *, #4571, .T. ) ;
#16081 = CARTESIAN_POINT ( 'NONE',  ( 211.3675436807652375, 27.51476459780207406, -13.34822117963639698 ) ) ;
#16082 = CARTESIAN_POINT ( 'NONE',  ( 197.7136026671465743, -1.979307457663559422, -11.01983352639493496 ) ) ;
#16083 = DIRECTION ( 'NONE',  ( -0.5000000000000049960, 0.8660254037844358210, -0.000000000000000000 ) ) ;
#16084 = CYLINDRICAL_SURFACE ( 'NONE', #14787, 3.902363844300889451 ) ;
#16085 = CARTESIAN_POINT ( 'NONE',  ( -27.63707102110206293, 9.448329371371865903, -4.575993311049476375 ) ) ;
#16086 = EDGE_LOOP ( 'NONE', ( #10090, #14717, #3827, #4495, #20851, #18399 ) ) ;
#16087 = LINE ( 'NONE', #4830, #8084 ) ;
#16088 = B_SPLINE_CURVE_WITH_KNOTS ( 'NONE', 3,
 ( #9553, #18040, #11571, #15938 ),
 .UNSPECIFIED., .F., .F.,
 ( 4, 4 ),
 ( 1.961874589857627478E-06, 0.0005678880968845024906 ),
 .UNSPECIFIED. ) ;
#16089 = ORIENTED_EDGE ( 'NONE', *, *, #6809, .T. ) ;
#16090 = CARTESIAN_POINT ( 'NONE',  ( 38.17255043510031953, 120.8395726428435637, -12.49999999999999822 ) ) ;
#16091 = EDGE_CURVE ( 'NONE', #7353, #19322, #12378, .T. ) ;
#16092 = CARTESIAN_POINT ( 'NONE',  ( -9.429792107721615579, 50.26201249766958057, -15.29528091781460297 ) ) ;
#16093 = FACE_OUTER_BOUND ( 'NONE', #12128, .T. ) ;
#16094 = DIRECTION ( 'NONE',  ( 0.8660254037844372643, 0.5000000000000027756, -0.000000000000000000 ) ) ;
#16095 = CARTESIAN_POINT ( 'NONE',  ( 97.13553065963888855, 198.8355456815907303, 12.25473482689746696 ) ) ;
#16096 = VECTOR ( 'NONE', #11630, 1000.000000000000000 ) ;
#16098 = ORIENTED_EDGE ( 'NONE', *, *, #2378, .T. ) ;
#16097 = ORIENTED_EDGE ( 'NONE', *, *, #5585, .T. ) ;
#16099 = EDGE_LOOP ( 'NONE', ( #20748, #14785, #17392, #6580, #13780, #19522, #1940 ) ) ;
#16100 = CARTESIAN_POINT ( 'NONE',  ( 218.9501057104153006, 10.79679952989121716, -16.84132998195102360 ) ) ;
#16101 = LINE ( 'NONE', #1567, #15965 ) ;
#16102 = CARTESIAN_POINT ( 'NONE',  ( -3.402542903551478926, 78.78634076744670267, -6.409256716261817033 ) ) ;
#16103 = EDGE_LOOP ( 'NONE', ( #4747, #13284, #9092, #10520 ) ) ;
#16104 = ORIENTED_EDGE ( 'NONE', *, *, #17565, .T. ) ;
#16105 = EDGE_LOOP ( 'NONE', ( #16631, #3412, #7546, #6731 ) ) ;
#16106 = EDGE_CURVE ( 'NONE', #17685, #4227, #7481, .T. ) ;
#16107 = CARTESIAN_POINT ( 'NONE',  ( -19.67995207262838520, 60.86351781624375690, -3.389291572743973635 ) ) ;
#16108 = DIRECTION ( 'NONE',  ( 0.8660254037844360431, 0.5000000000000044409, -5.976026924694053325E-17 ) ) ;
#16109 = CARTESIAN_POINT ( 'NONE',  ( 31.01452848080070268, 210.2376303493833234, -14.00000000000002842 ) ) ;
#16110 = CARTESIAN_POINT ( 'NONE',  ( 0.000000000000000000, 0.000000000000000000, 0.000000000000000000 ) ) ;
#16111 = VERTEX_POINT ( 'NONE', #13975 ) ;
#16112 = VERTEX_POINT ( 'NONE', #12691 ) ;
#16113 = CARTESIAN_POINT ( 'NONE',  ( 201.7914626300884890, 0.3750460896586316206, -22.62267072728657524 ) ) ;
#16114 = CIRCLE ( 'NONE', #14085, 11.94520687646042667 ) ;
#16115 = VECTOR ( 'NONE', #13587, 1000.000000000000227 ) ;
#16116 = LINE ( 'NONE', #6229, #14217 ) ;
#16117 = EDGE_CURVE ( 'NONE', #12336, #15178, #12480, .T. ) ;
#16118 = LINE ( 'NONE', #8025, #1085 ) ;
#16119 = CARTESIAN_POINT ( 'NONE',  ( -27.74827478545477888, 57.32317209004575176, 4.280504417503601111 ) ) ;
#16120 = DIRECTION ( 'NONE',  ( 0.5000000000000055511, -0.8660254037844353769, 1.110223024625156417E-16 ) ) ;
#16121 = CARTESIAN_POINT ( 'NONE',  ( 201.8234976231972553, 26.52995303002162331, -14.00000000000004619 ) ) ;
#16122 = DIRECTION ( 'NONE',  ( 0.000000000000000000, 1.000000000000000000, 0.000000000000000000 ) ) ;
#16123 = DIRECTION ( 'NONE',  ( -0.000000000000000000, -1.000000000000000000, -0.000000000000000000 ) ) ;
#16124 = ORIENTED_EDGE ( 'NONE', *, *, #9505, .T. ) ;
#16125 = AXIS2_PLACEMENT_3D ( 'NONE', #13838, #2909, #12248 ) ;
#16126 = CARTESIAN_POINT ( 'NONE',  ( 62.63374148850010670, 78.15280783560238831, -9.335207922937284408 ) ) ;
#16127 = EDGE_CURVE ( 'NONE', #7288, #10818, #15776, .T. ) ;
#16128 = EDGE_LOOP ( 'NONE', ( #13915, #9763, #2377, #14875 ) ) ;
#16129 = AXIS2_PLACEMENT_3D ( 'NONE', #11661, #3692, #2014 ) ;
#16130 = EDGE_CURVE ( 'NONE', #3527, #14413, #8384, .T. ) ;
#16131 = ORIENTED_EDGE ( 'NONE', *, *, #11730, .F. ) ;
#16132 = LINE ( 'NONE', #529, #9821 ) ;
#16133 = CIRCLE ( 'NONE', #7649, 3.902363844300875240 ) ;
#16134 = LINE ( 'NONE', #13149, #11710 ) ;
#16135 = CARTESIAN_POINT ( 'NONE',  ( 5.000000000000004441, 2.815456201510357988E-17, 4.057500000000029416 ) ) ;
#16136 = ADVANCED_FACE ( 'NONE', ( #6089 ), #20312, .F. ) ;
#16137 = VERTEX_POINT ( 'NONE', #4522 ) ;
#16138 = CIRCLE ( 'NONE', #6972, 4.999999999999989342 ) ;
#16139 = PLANE ( 'NONE',  #20932 ) ;
#16140 = CARTESIAN_POINT ( 'NONE',  ( 209.9065677398659204, 29.65222043997809109, -16.50006186076872083 ) ) ;
#16141 = LINE ( 'NONE', #4782, #19335 ) ;
#16142 = AXIS2_PLACEMENT_3D ( 'NONE', #10443, #5674, #20106 ) ;
#16143 = CARTESIAN_POINT ( 'NONE',  ( 48.48114019555096377, 209.9845714233581191, 45.12705109663953351 ) ) ;
#16144 = DIRECTION ( 'NONE',  ( 0.8660254037844357100, 0.5000000000000052180, 0.000000000000000000 ) ) ;
#16145 = CONICAL_SURFACE ( 'NONE', #5960, 4.509097725792825528, 0.5235987755983015912 ) ;
#16146 = EDGE_CURVE ( 'NONE', #9864, #18037, #20415, .T. ) ;
#16147 = DIRECTION ( 'NONE',  ( 7.930164461608273850E-15, 3.965082230804136925E-15, -1.000000000000000000 ) ) ;
#16148 = DIRECTION ( 'NONE',  ( -0.8660254037844358210, -0.5000000000000049960, 0.000000000000000000 ) ) ;
#16149 = CARTESIAN_POINT ( 'NONE',  ( 198.0096515360099261, -1.293177324654909643, -12.56699194733486280 ) ) ;
#16150 = ORIENTED_EDGE ( 'NONE', *, *, #10063, .T. ) ;
#16151 = CARTESIAN_POINT ( 'NONE',  ( 221.1184916184598706, 33.44636523676208384, -11.01522019104625372 ) ) ;
#16152 = EDGE_CURVE ( 'NONE', #16560, #7294, #17140, .T. ) ;
#16153 = CARTESIAN_POINT ( 'NONE',  ( 10.49211908931699178, 0.000000000000000000, 0.000000000000000000 ) ) ;
#16154 = DIRECTION ( 'NONE',  ( -0.000000000000000000, -0.000000000000000000, -1.000000000000000000 ) ) ;
#16155 = CARTESIAN_POINT ( 'NONE',  ( -28.48915680482255652, 80.00000000000000000, 0.5205403966592361265 ) ) ;
#16157 = ORIENTED_EDGE ( 'NONE', *, *, #2283, .F. ) ;
#16156 = ORIENTED_EDGE ( 'NONE', *, *, #19650, .F. ) ;
#16158 = DIRECTION ( 'NONE',  ( 0.8645602258681719388, 0.4991540791356394169, 0.05814482891046558050 ) ) ;
#16159 = PRODUCT_DEFINITION_CONTEXT ( 'detailed design', #1206, 'design' ) ;
#16160 = ORIENTED_EDGE ( 'NONE', *, *, #10561, .F. ) ;
#16161 = EDGE_CURVE ( 'NONE', #9686, #8683, #7662, .T. ) ;
#16162 = CARTESIAN_POINT ( 'NONE',  ( -31.96408918797520471, 67.75983095507351095, 2.252573492070595318 ) ) ;
#16163 = EDGE_CURVE ( 'NONE', #9470, #6339, #15816, .T. ) ;
#16164 = ORIENTED_EDGE ( 'NONE', *, *, #17990, .F. ) ;
#16165 = LINE ( 'NONE', #1631, #9620 ) ;
#16166 = ORIENTED_EDGE ( 'NONE', *, *, #3686, .T. ) ;
#16167 = LINE ( 'NONE', #19430, #10549 ) ;
#16168 = ADVANCED_FACE ( 'NONE', ( #7584 ), #2833, .F. ) ;
#16169 = CARTESIAN_POINT ( 'NONE',  ( 76.66199489384241872, 68.03321850950067073, 0.1432382234697572587 ) ) ;
#16170 = VECTOR ( 'NONE', #13681, 1000.000000000000227 ) ;
#16171 = CARTESIAN_POINT ( 'NONE',  ( 0.000000000000000000, 1.759474945355379960, -3.047500000000001652 ) ) ;
#16172 = ORIENTED_EDGE ( 'NONE', *, *, #277, .F. ) ;
#16173 = CARTESIAN_POINT ( 'NONE',  ( 0.000000000000000000, -2.342598717236899830, 4.057500000000059615 ) ) ;
#16175 = DIRECTION ( 'NONE',  ( -0.5000000000000049960, 0.8660254037844358210, -0.000000000000000000 ) ) ;
#16174 = VECTOR ( 'NONE', #20608, 1000.000000000000227 ) ;
#16176 = ORIENTED_EDGE ( 'NONE', *, *, #17676, .F. ) ;
#16177 = DIRECTION ( 'NONE',  ( -1.000000000000000000, -0.000000000000000000, -0.000000000000000000 ) ) ;
#16178 = EDGE_CURVE ( 'NONE', #2244, #12371, #160, .T. ) ;
#16179 = B_SPLINE_CURVE_WITH_KNOTS ( 'NONE', 3,
 ( #5839, #15524, #9325, #1090 ),
 .UNSPECIFIED., .F., .F.,
 ( 4, 4 ),
 ( 2.304444449537611917E-05, 0.0005889706667902999161 ),
 .UNSPECIFIED. ) ;
#16180 = ORIENTED_EDGE ( 'NONE', *, *, #8372, .T. ) ;
#16181 = CARTESIAN_POINT ( 'NONE',  ( 209.4060512283256230, 30.62413204007591716, -11.83134160488075715 ) ) ;
#16182 = PLANE ( 'NONE',  #1737 ) ;
#16183 = CARTESIAN_POINT ( 'NONE',  ( 28.51452848080068847, 214.5677573683055357, -14.00000000000002842 ) ) ;
#16184 = CARTESIAN_POINT ( 'NONE',  ( 227.9553588074475954, 39.88513931160571957, -14.00000000000005507 ) ) ;
#16185 = DIRECTION ( 'NONE',  ( 0.000000000000000000, 0.000000000000000000, -1.000000000000000000 ) ) ;
#16186 = ORIENTED_EDGE ( 'NONE', *, *, #14045, .F. ) ;
#16187 = CIRCLE ( 'NONE', #2309, 12.47473710546057823 ) ;
#16188 = CARTESIAN_POINT ( 'NONE',  ( 70.88961965102326701, 73.20066112274578529, -22.81645270491783251 ) ) ;
#16189 = CARTESIAN_POINT ( 'NONE',  ( 201.5034618240616453, 7.454766308978539868, -25.15316579317382306 ) ) ;
#16190 = ORIENTED_EDGE ( 'NONE', *, *, #15143, .F. ) ;
#16191 = CARTESIAN_POINT ( 'NONE',  ( 225.9328258572189725, 42.73531000888135623, -15.54732812283875454 ) ) ;
#16192 = CARTESIAN_POINT ( 'NONE',  ( -0.2021197016317256845, 50.46427967968534034, -8.782110831005875085 ) ) ;
#16193 = DIRECTION ( 'NONE',  ( -0.5000000000000049960, 0.8660254037844358210, -0.000000000000000000 ) ) ;
#16194 = CARTESIAN_POINT ( 'NONE',  ( 227.9553588074475954, 39.88513931160571957, -14.00000000000005507 ) ) ;
#16195 = CARTESIAN_POINT ( 'NONE',  ( 97.97877128586738138, 199.4920122637983297, 13.24606046902644074 ) ) ;
#16197 = EDGE_LOOP ( 'NONE', ( #14887, #1640, #16870, #2495 ) ) ;
#16196 = ORIENTED_EDGE ( 'NONE', *, *, #9637, .T. ) ;
#16198 = DIRECTION ( 'NONE',  ( 0.4999999999999995004, -0.8660254037844390407, 0.000000000000000000 ) ) ;
#16199 = CARTESIAN_POINT ( 'NONE',  ( -13.40786934824189558, 79.99957779460261520, -12.37049764041790390 ) ) ;
#16200 = ORIENTED_EDGE ( 'NONE', *, *, #435, .T. ) ;
#16201 = ORIENTED_EDGE ( 'NONE', *, *, #8968, .F. ) ;
#16202 = DIRECTION ( 'NONE',  ( 0.8660254037844377084, 0.5000000000000017764, -1.040834085586084380E-16 ) ) ;
#16203 = CARTESIAN_POINT ( 'NONE',  ( 228.0752873022257461, 39.67741706537471913, -17.89498551959672668 ) ) ;
#16204 = CARTESIAN_POINT ( 'NONE',  ( 195.0230325291159090, 3.359249353468287680, -14.01558723443171850 ) ) ;
#16205 = CARTESIAN_POINT ( 'NONE',  ( 227.8089867185126991, 40.13866320645093566, -10.39224118001587449 ) ) ;
#16206 = ORIENTED_EDGE ( 'NONE', *, *, #13024, .T. ) ;
#16207 = ORIENTED_EDGE ( 'NONE', *, *, #3706, .T. ) ;
#16208 = PLANE ( 'NONE',  #20876 ) ;
#16209 = VECTOR ( 'NONE', #17108, 1000.000000000000000 ) ;
#16210 = DIRECTION ( 'NONE',  ( 0.5000000000000049960, -0.8660254037844358210, 0.000000000000000000 ) ) ;
#16211 = ADVANCED_FACE ( 'NONE', ( #13102 ), #14708, .F. ) ;
#16212 = DIRECTION ( 'NONE',  ( -0.000000000000000000, -1.000000000000000000, -0.000000000000000000 ) ) ;
#16213 = DIRECTION ( 'NONE',  ( 0.8660254037844362651, 0.5000000000000039968, -0.000000000000000000 ) ) ;
#16214 = PLANE ( 'NONE',  #19074 ) ;
#16215 = CARTESIAN_POINT ( 'NONE',  ( 203.4811056270561664, 23.51224104295614481, -25.46066938576263894 ) ) ;
#16216 = LINE ( 'NONE', #3375, #17813 ) ;
#16217 = ORIENTED_EDGE ( 'NONE', *, *, #18216, .F. ) ;
#16218 = CARTESIAN_POINT ( 'NONE',  ( 55.93063010822693570, 77.28382646649683352, -8.238606096522689271 ) ) ;
#16219 = VERTEX_POINT ( 'NONE', #1448 ) ;
#16220 = AXIS2_PLACEMENT_3D ( 'NONE', #17515, #9433, #16042 ) ;
#16221 = DIRECTION ( 'NONE',  ( -2.645739781067712995E-16, -1.527518574805166670E-16, -1.000000000000000000 ) ) ;
#16222 = PLANE ( 'NONE',  #877 ) ;
#16223 = EDGE_CURVE ( 'NONE', #5368, #3353, #11190, .T. ) ;
#16224 = ORIENTED_EDGE ( 'NONE', *, *, #4691, .F. ) ;
#16225 = DIRECTION ( 'NONE',  ( 0.5000000000000044409, -0.8660254037844360431, -4.006172263299080068E-16 ) ) ;
#16226 = LINE ( 'NONE', #14449, #6201 ) ;
#16227 = EDGE_LOOP ( 'NONE', ( #15265, #6480, #4296, #16027 ) ) ;
#16228 = CARTESIAN_POINT ( 'NONE',  ( 218.6685935962727001, 37.89566518712205578, -16.41980614534970684 ) ) ;
#16229 = FACE_OUTER_BOUND ( 'NONE', #2910, .T. ) ;
#16230 = CARTESIAN_POINT ( 'NONE',  ( 194.9478548255267754, 18.58556639563049018, -25.46066938576250038 ) ) ;
#16231 = EDGE_CURVE ( 'NONE', #3522, #14639, #11747, .T. ) ;
#16232 = AXIS2_PLACEMENT_3D ( 'NONE', #7374, #12284, #7175 ) ;
#16233 = EDGE_CURVE ( 'NONE', #14889, #12331, #17669, .T. ) ;
#16234 = CARTESIAN_POINT ( 'NONE',  ( 215.9040783327276358, 15.94597603093701466, -15.40420431385954281 ) ) ;
#16235 = CARTESIAN_POINT ( 'NONE',  ( 221.1274251996601663, 33.84282198876892522, -17.45257705044835816 ) ) ;
#16236 = DIRECTION ( 'NONE',  ( 0.5000000000000007772, -0.8660254037844381525, 0.000000000000000000 ) ) ;
#16237 = CYLINDRICAL_SURFACE ( 'NONE', #10248, 5.000000000000036415 ) ;
#16238 = LINE ( 'NONE', #130, #2074 ) ;
#16239 = VERTEX_POINT ( 'NONE', #18075 ) ;
#16240 = VERTEX_POINT ( 'NONE', #19441 ) ;
#16241 = CARTESIAN_POINT ( 'NONE',  ( 215.7530533430368394, 15.85878171248467439, -16.01416015924714742 ) ) ;
#16242 = AXIS2_PLACEMENT_3D ( 'NONE', #5667, #10226, #15047 ) ;
#16243 = CARTESIAN_POINT ( 'NONE',  ( 58.57586221349182409, 85.50000000000065370, -12.24792819076230366 ) ) ;
#16244 = DIRECTION ( 'NONE',  ( 0.5000000000000051070, -0.8660254037844359321, 0.000000000000000000 ) ) ;
#16245 = CARTESIAN_POINT ( 'NONE',  ( 79.46180180641687230, 49.77667888093298387, -9.984653723550882987 ) ) ;
#16246 = APPLICATION_CONTEXT ( 'automotive_design' ) ;
#16248 = ORIENTED_EDGE ( 'NONE', *, *, #1932, .F. ) ;
#16247 = ORIENTED_EDGE ( 'NONE', *, *, #20624, .F. ) ;
#16249 = VECTOR ( 'NONE', #18475, 1000.000000000000227 ) ;
#16250 = FACE_OUTER_BOUND ( 'NONE', #11218, .T. ) ;
#16251 = ORIENTED_EDGE ( 'NONE', *, *, #7828, .T. ) ;
#16252 = EDGE_CURVE ( 'NONE', #17368, #2011, #3603, .T. ) ;
#16253 = VECTOR ( 'NONE', #1873, 1000.000000000000114 ) ;
#16254 = DIRECTION ( 'NONE',  ( 0.000000000000000000, 0.5134338004640807140, 0.8581292050390840753 ) ) ;
#16255 = DIRECTION ( 'NONE',  ( 0.8660254037844373753, 0.5000000000000022204, -6.661338147750940229E-16 ) ) ;
#16256 = CARTESIAN_POINT ( 'NONE',  ( 218.9947030324160835, 37.12487497232478262, -17.03266613944931862 ) ) ;
#16257 = EDGE_LOOP ( 'NONE', ( #3991, #10201, #7615, #13454 ) ) ;
#16258 = EDGE_CURVE ( 'NONE', #10070, #17532, #17258, .T. ) ;
#16259 = CARTESIAN_POINT ( 'NONE',  ( 205.0662616026534693, 10.91332106064940888, -14.00000000000005507 ) ) ;
#16260 = ADVANCED_FACE ( 'NONE', ( #14396 ), #9689, .T. ) ;
#16261 = CARTESIAN_POINT ( 'NONE',  ( 57.73559688320084149, 76.51496841747558619, -6.433815121522095559 ) ) ;
#16262 = CARTESIAN_POINT ( 'NONE',  ( -29.55307521651278435, 64.25000000000002842, 3.020008312198915412 ) ) ;
#16264 = EDGE_CURVE ( 'NONE', #5922, #11617, #1754, .T. ) ;
#16263 = ORIENTED_EDGE ( 'NONE', *, *, #2110, .F. ) ;
#16265 = CARTESIAN_POINT ( 'NONE',  ( 220.2180084519553134, 35.41797800104779270, -14.00000000000005507 ) ) ;
#16266 = LINE ( 'NONE', #1542, #5408 ) ;
#16267 = ADVANCED_FACE ( 'NONE', ( #14497 ), #19251, .T. ) ;
#16268 = ORIENTED_EDGE ( 'NONE', *, *, #3457, .F. ) ;
#16269 = FACE_OUTER_BOUND ( 'NONE', #645, .T. ) ;
#16270 = AXIS2_PLACEMENT_3D ( 'NONE', #14548, #116, #6652 ) ;
#16271 = ORIENTED_EDGE ( 'NONE', *, *, #9368, .F. ) ;
#16272 = CARTESIAN_POINT ( 'NONE',  ( 210.8927598318763899, 28.12706523984405038, -12.11611233826046963 ) ) ;
#16273 = CARTESIAN_POINT ( 'NONE',  ( 220.5312744984369431, 34.66940722628535099, -17.70629034850377792 ) ) ;
#16274 = CARTESIAN_POINT ( 'NONE',  ( 220.1445873793223598, 35.13321686065494021, -17.67703110843607917 ) ) ;
#16275 = VECTOR ( 'NONE', #10244, 1000.000000000000227 ) ;
#16276 = EDGE_CURVE ( 'NONE', #1882, #16846, #8352, .T. ) ;
#16277 = SHAPE_REPRESENTATION ( '60-Degree Angle Clamping Handle', ( #18233 ), #16874 ) ;
#16278 = CIRCLE ( 'NONE', #10508, 4.057500000000029416 ) ;
#16279 = DIRECTION ( 'NONE',  ( -0.8660254037844370423, -0.5000000000000026645, 0.000000000000000000 ) ) ;
#16280 = PLANE ( 'NONE',  #17192 ) ;
#16281 = AXIS2_PLACEMENT_3D ( 'NONE', #5293, #11679, #14679 ) ;
#16282 = CARTESIAN_POINT ( 'NONE',  ( 82.49529059433407951, 181.0703347563770365, 16.00000000000001066 ) ) ;
#16283 = VERTEX_POINT ( 'NONE', #17974 ) ;
#16284 = VECTOR ( 'NONE', #4793, 1000.000000000000000 ) ;
#16285 = CARTESIAN_POINT ( 'NONE',  ( 76.78232915647551238, 69.44169262812657450, -24.77272969115283274 ) ) ;
#16286 = EDGE_CURVE ( 'NONE', #15417, #6104, #20865, .T. ) ;
#16287 = CARTESIAN_POINT ( 'NONE',  ( -4.681704537686387724, 62.69813775908227171, 5.305497683706574819 ) ) ;
#16288 = EDGE_CURVE ( 'NONE', #2452, #15788, #16473, .T. ) ;
#16289 = CIRCLE ( 'NONE', #7133, 11.94520687646042667 ) ;
#16290 = EDGE_LOOP ( 'NONE', ( #3661, #8728, #3874, #13030 ) ) ;
#16291 = CARTESIAN_POINT ( 'NONE',  ( 50.60228022274853288, 140.3106491262845736, 41.00000000000001421 ) ) ;
#16292 = CARTESIAN_POINT ( 'NONE',  ( -4.343379421876969460, 58.21999429253379077, 4.515609508575330722 ) ) ;
#16293 = LINE ( 'NONE', #3350, #16707 ) ;
#16294 = EDGE_CURVE ( 'NONE', #2546, #18365, #5973, .T. ) ;
#16295 = DIRECTION ( 'NONE',  ( -0.000000000000000000, -0.000000000000000000, 1.000000000000000000 ) ) ;
#16296 = VECTOR ( 'NONE', #15748, 1000.000000000000000 ) ;
#16297 = DIRECTION ( 'NONE',  ( 0.8660254037844355990, 0.5000000000000054401, 8.899770914925154148E-15 ) ) ;
#16298 = EDGE_CURVE ( 'NONE', #15249, #15363, #1831, .T. ) ;
#16300 = ORIENTED_EDGE ( 'NONE', *, *, #10569, .T. ) ;
#16299 = ORIENTED_EDGE ( 'NONE', *, *, #7824, .F. ) ;
#16301 = ORIENTED_EDGE ( 'NONE', *, *, #15456, .T. ) ;
#16302 = LINE ( 'NONE', #19673, #1728 ) ;
#16304 = CARTESIAN_POINT ( 'NONE',  ( 219.8340134144083606, 36.08307691593343236, -10.17395310825081189 ) ) ;
#16303 = AXIS2_PLACEMENT_3D ( 'NONE', #14075, #19145, #4619 ) ;
#16305 = EDGE_CURVE ( 'NONE', #14290, #18515, #14811, .T. ) ;
#16306 = CIRCLE ( 'NONE', #5783, 1.000000000000000888 ) ;
#16307 = ORIENTED_EDGE ( 'NONE', *, *, #14975, .T. ) ;
#16308 = ORIENTED_EDGE ( 'NONE', *, *, #8622, .T. ) ;
#16309 = LINE ( 'NONE', #15948, #8859 ) ;
#16310 = DIRECTION ( 'NONE',  ( 0.5000000000000054401, -0.8660254037844353769, 3.330669073875469128E-16 ) ) ;
#16311 = CARTESIAN_POINT ( 'NONE',  ( 4.000000000000000000, -2.639212418033072716, 1.523750000000001492 ) ) ;
#16312 = LINE ( 'NONE', #11325, #6291 ) ;
#16313 = ORIENTED_EDGE ( 'NONE', *, *, #9749, .T. ) ;
#16314 = EDGE_CURVE ( 'NONE', #12179, #10014, #14242, .T. ) ;
#16315 = VERTEX_POINT ( 'NONE', #260 ) ;
#16316 = DIRECTION ( 'NONE',  ( -0.8660254037844370423, -0.5000000000000026645, 0.000000000000000000 ) ) ;
#16317 = AXIS2_PLACEMENT_3D ( 'NONE', #13641, #12151, #7574 ) ;
#16318 = CARTESIAN_POINT ( 'NONE',  ( 190.9712048706970506, 36.57158503910383729, -18.97089895516968028 ) ) ;
#16319 = EDGE_CURVE ( 'NONE', #20139, #9718, #10095, .T. ) ;
#16320 = AXIS2_PLACEMENT_3D ( 'NONE', #16696, #8522, #15022 ) ;
#16321 = CONICAL_SURFACE ( 'NONE', #20034, 13.07248899748297433, 0.6693469023067423196 ) ;
#16322 = CARTESIAN_POINT ( 'NONE',  ( 210.0930887352476759, 12.05995036078138583, -25.46066938576263894 ) ) ;
#16323 = CARTESIAN_POINT ( 'NONE',  ( 5.000000000000004441, -3.513898075855361736, -2.028750000000006715 ) ) ;
#16324 = DIRECTION ( 'NONE',  ( 0.000000000000000000, 0.4999999999999985012, -0.8660254037844394848 ) ) ;
#16325 = ORIENTED_EDGE ( 'NONE', *, *, #1890, .T. ) ;
#16326 = DIRECTION ( 'NONE',  ( -0.5000000000000049960, 0.8660254037844357100, -0.000000000000000000 ) ) ;
#16327 = LINE ( 'NONE', #4869, #5534 ) ;
#16328 = ORIENTED_EDGE ( 'NONE', *, *, #11344, .T. ) ;
#16329 = CARTESIAN_POINT ( 'NONE',  ( 68.95169418938438355, 77.46545255404963370, -2.018454592414399951 ) ) ;
#16330 = EDGE_LOOP ( 'NONE', ( #4560, #14594, #1625, #15555 ) ) ;
#16331 = CARTESIAN_POINT ( 'NONE',  ( 218.9129779831750682, 10.51775681150463448, -11.19970074074921662 ) ) ;
#16332 = DIRECTION ( 'NONE',  ( 0.000000000000000000, -0.4999999999999983902, 0.8660254037844394848 ) ) ;
#16333 = AXIS2_PLACEMENT_3D ( 'NONE', #3731, #15322, #20066 ) ;
#16334 = AXIS2_PLACEMENT_3D ( 'NONE', #4215, #13869, #15781 ) ;
#16335 = EDGE_CURVE ( 'NONE', #11067, #7909, #5635, .T. ) ;
#16336 = VERTEX_POINT ( 'NONE', #18391 ) ;
#16337 = DIRECTION ( 'NONE',  ( 0.8660254037844370423, 0.5000000000000026645, -0.000000000000000000 ) ) ;
#16338 = VERTEX_POINT ( 'NONE', #2070 ) ;
#16339 = FACE_OUTER_BOUND ( 'NONE', #11568, .T. ) ;
#16340 = EDGE_LOOP ( 'NONE', ( #13964, #6406, #17779, #7507, #10546 ) ) ;
#16341 = CARTESIAN_POINT ( 'NONE',  ( 63.15554463217812042, 234.5677573683057062, -19.00000000000000355 ) ) ;
#16342 = FACE_OUTER_BOUND ( 'NONE', #12115, .T. ) ;
#16343 = DIRECTION ( 'NONE',  ( 0.9679941405060890069, 0.000000000000000000, -0.2509727952306343712 ) ) ;
#16344 = DIRECTION ( 'NONE',  ( -0.8660254037844355990, -0.5000000000000054401, -1.154189040529355901E-14 ) ) ;
#16345 = VECTOR ( 'NONE', #3921, 1000.000000000000000 ) ;
#16346 = ORIENTED_EDGE ( 'NONE', *, *, #12803, .F. ) ;
#16347 = FACE_OUTER_BOUND ( 'NONE', #8205, .T. ) ;
#16348 = ADVANCED_FACE ( 'NONE', ( #12032 ), #11928, .T. ) ;
#16349 = AXIS2_PLACEMENT_3D ( 'NONE', #3857, #682, #18176 ) ;
#16350 = DIRECTION ( 'NONE',  ( -0.5000000000000049960, 0.8660254037844358210, -0.000000000000000000 ) ) ;
#16351 = CARTESIAN_POINT ( 'NONE',  ( 205.8264633344831225, 9.596613037118636669, -14.00000000000005507 ) ) ;
#16352 = ORIENTED_EDGE ( 'NONE', *, *, #162, .F. ) ;
#16353 = DIRECTION ( 'NONE',  ( 0.000000000000000000, 0.000000000000000000, 1.000000000000000000 ) ) ;
#16354 = CARTESIAN_POINT ( 'NONE',  ( 68.41618888151715794, 77.88480544091760294, -2.239802524522644944 ) ) ;
#16355 = DIRECTION ( 'NONE',  ( 0.8660254037844352659, 0.5000000000000056621, 0.000000000000000000 ) ) ;
#16356 = CARTESIAN_POINT ( 'NONE',  ( 79.66622197694607621, 50.33767513494625945, -16.74958941344072016 ) ) ;
#16358 = ORIENTED_EDGE ( 'NONE', *, *, #13422, .T. ) ;
#16357 = ORIENTED_EDGE ( 'NONE', *, *, #17815, .T. ) ;
#16359 = ADVANCED_FACE ( 'NONE', ( #3641 ), #907, .F. ) ;
#16360 = VERTEX_POINT ( 'NONE', #10306 ) ;
#16361 = UNCERTAINTY_MEASURE_WITH_UNIT (LENGTH_MEASURE( 1.000000000000000082E-05 ), #12219, 'distance_accuracy_value', 'NONE');
#16362 = EDGE_LOOP ( 'NONE', ( #4191, #12402, #11287, #14714 ) ) ;
#16363 = AXIS2_PLACEMENT_3D ( 'NONE', #9102, #14122, #7626 ) ;
#16364 = CARTESIAN_POINT ( 'NONE',  ( 190.7433706042750146, 35.72129598111152404, -9.000000000000062172 ) ) ;
#16365 = ORIENTED_EDGE ( 'NONE', *, *, #14210, .T. ) ;
#16366 = SURFACE_STYLE_USAGE ( .BOTH. , #6584 ) ;
#16367 = CARTESIAN_POINT ( 'NONE',  ( 195.4369152048313367, 3.952243985314471075, -11.19512133156234057 ) ) ;
#16368 = ORIENTED_EDGE ( 'NONE', *, *, #2685, .F. ) ;
#16369 = DIRECTION ( 'NONE',  ( 0.000000000000000000, 1.000000000000000000, 0.000000000000000000 ) ) ;
#16370 = CARTESIAN_POINT ( 'NONE',  ( 55.07002310602048567, 77.64981942332057940, -15.50454273085438928 ) ) ;
#16371 = LINE ( 'NONE', #3734, #942 ) ;
#16372 = ORIENTED_EDGE ( 'NONE', *, *, #8756, .T. ) ;
#16373 = APPLICATION_CONTEXT ( 'automotive_design' ) ;
#16374 = AXIS2_PLACEMENT_3D ( 'NONE', #9334, #15244, #13530 ) ;
#16375 =( NAMED_UNIT ( * ) SI_UNIT ( $, .STERADIAN. ) SOLID_ANGLE_UNIT ( ) );
#16376 = CARTESIAN_POINT ( 'NONE',  ( 203.9371734008334158, 8.505830985348726614, -1.717498466822810599 ) ) ;
#16377 = ORIENTED_EDGE ( 'NONE', *, *, #6874, .F. ) ;
#16378 = DIRECTION ( 'NONE',  ( 0.8660254037844372643, 0.5000000000000023315, 6.106226635438360972E-16 ) ) ;
#16379 = EDGE_CURVE ( 'NONE', #4599, #16542, #16800, .T. ) ;
#16380 = ORIENTED_EDGE ( 'NONE', *, *, #17445, .F. ) ;
#16381 = ADVANCED_FACE ( 'NONE', ( #16584 ), #15338, .F. ) ;
#16382 = DIRECTION ( 'NONE',  ( -0.8660254037844349329, -0.5000000000000064393, 0.000000000000000000 ) ) ;
#16383 = DIRECTION ( 'NONE',  ( 3.965082230804136136E-15, 7.930164461608272272E-15, 1.000000000000000000 ) ) ;
#16384 = CARTESIAN_POINT ( 'NONE',  ( 208.8107687779841228, 4.427644383670616079, -14.00000000000005507 ) ) ;
#16385 = FACE_OUTER_BOUND ( 'NONE', #17111, .T. ) ;
#16386 = CARTESIAN_POINT ( 'NONE',  ( -26.20384780446736173, 9.999999997039491717, -7.228202927376838893 ) ) ;
#16387 = CIRCLE ( 'NONE', #19746, 4.999999999999999112 ) ;
#16388 = AXIS2_PLACEMENT_3D ( 'NONE', #19213, #13063, #16148 ) ;
#16389 = DIRECTION ( 'NONE',  ( 0.8660254037844369313, 0.5000000000000029976, 3.053113317719180486E-16 ) ) ;
#16390 = ORIENTED_EDGE ( 'NONE', *, *, #2684, .T. ) ;
#16391 = EDGE_CURVE ( 'NONE', #13972, #15690, #3276, .T. ) ;
#16392 = CARTESIAN_POINT ( 'NONE',  ( 74.22444910852603073, 69.25129922422347306, -24.80018073758580854 ) ) ;
#16393 = CARTESIAN_POINT ( 'NONE',  ( -3.848310109324514006, 46.83026313486608672, -2.948019393338978222 ) ) ;
#16394 = ORIENTED_EDGE ( 'NONE', *, *, #9871, .T. ) ;
#16395 = CARTESIAN_POINT ( 'NONE',  ( 227.9553588074475954, 39.88513931160571957, -14.00000000000005507 ) ) ;
#16396 = CARTESIAN_POINT ( 'NONE',  ( -3.651764899804558429, 52.03701157797662091, 1.955602390459402873 ) ) ;
#16397 = DIRECTION ( 'NONE',  ( 0.000000000000000000, -1.000000000000000000, -3.469446951953589044E-16 ) ) ;
#16398 = EDGE_CURVE ( 'NONE', #12398, #3941, #5544, .T. ) ;
#16399 = CARTESIAN_POINT ( 'NONE',  ( 207.8872982515397609, 15.44148381043179263, -24.85758746085098991 ) ) ;
#16400 = LINE ( 'NONE', #599, #18796 ) ;
#16402 = ORIENTED_EDGE ( 'NONE', *, *, #13702, .F. ) ;
#16401 = ORIENTED_EDGE ( 'NONE', *, *, #675, .F. ) ;
#16403 = VERTEX_POINT ( 'NONE', #10415 ) ;
#16404 = AXIS2_PLACEMENT_3D ( 'NONE', #8737, #18181, #10421 ) ;
#16405 = PLANE ( 'NONE',  #10155 ) ;
#16406 = CARTESIAN_POINT ( 'NONE',  ( -15.99999999999999289, -9.999999999999994671, 0.000000000000000000 ) ) ;
#16407 = ADVANCED_FACE ( 'NONE', ( #16900 ), #10021, .T. ) ;
#16408 = ORIENTED_EDGE ( 'NONE', *, *, #2260, .F. ) ;
#16409 = CARTESIAN_POINT ( 'NONE',  ( 96.88087538439037871, 198.6134603144003563, 11.00000000000000888 ) ) ;
#16410 = CARTESIAN_POINT ( 'NONE',  ( 104.3328820505367531, 188.7062061502930135, 11.00000000000001066 ) ) ;
#16411 = CARTESIAN_POINT ( 'NONE',  ( 79.36131599811857029, 188.4985379866525932, 11.00000000000001066 ) ) ;
#16412 = CARTESIAN_POINT ( 'NONE',  ( -13.69112006203626564, 59.06815658944699976, -4.446547635559181977 ) ) ;
#16413 = VERTEX_POINT ( 'NONE', #19964 ) ;
#16414 = ORIENTED_EDGE ( 'NONE', *, *, #18615, .F. ) ;
#16415 = CARTESIAN_POINT ( 'NONE',  ( 199.3871399495608898, 6.055890627870659237, -23.87887634647626101 ) ) ;
#16416 = EDGE_CURVE ( 'NONE', #2244, #19879, #15161, .T. ) ;
#16417 = ORIENTED_EDGE ( 'NONE', *, *, #3467, .T. ) ;
#16418 = EDGE_CURVE ( 'NONE', #10811, #10118, #17000, .T. ) ;
#16419 = CIRCLE ( 'NONE', #15422, 12.47473710546057823 ) ;
#16420 = DIRECTION ( 'NONE',  ( 0.5000000000000057732, -0.8660254037844353769, 0.000000000000000000 ) ) ;
#16421 = DIRECTION ( 'NONE',  ( 0.3654179821390598493, -0.6329225110641440999, 0.6825531432186625613 ) ) ;
#16422 = CARTESIAN_POINT ( 'NONE',  ( -28.28208682648537220, 52.78748761784272148, -3.776222344276643827 ) ) ;
#16423 = CARTESIAN_POINT ( 'NONE',  ( 206.3644977982345665, 10.08427006003479853, -1.709088388254546675 ) ) ;
#16424 = EDGE_CURVE ( 'NONE', #6609, #8072, #19535, .T. ) ;
#16425 = CARTESIAN_POINT ( 'NONE',  ( 157.3972143829815309, 45.33639716978957068, -22.00000000000007816 ) ) ;
#16426 = DIRECTION ( 'NONE',  ( -0.5000000000000049960, 0.8660254037844357100, -0.000000000000000000 ) ) ;
#16427 = ORIENTED_EDGE ( 'NONE', *, *, #3841, .F. ) ;
#16428 = CARTESIAN_POINT ( 'NONE',  ( 54.56775351867148771, 77.86323848837362505, -10.60172925492977214 ) ) ;
#16429 = ORIENTED_EDGE ( 'NONE', *, *, #5574, .T. ) ;
#16430 = CARTESIAN_POINT ( 'NONE',  ( 208.0983737146324870, 5.661548828456886895, -14.00000000000005507 ) ) ;
#16431 = FACE_OUTER_BOUND ( 'NONE', #3476, .T. ) ;
#16432 = ADVANCED_FACE ( 'NONE', ( #20390 ), #19197, .F. ) ;
#16433 = CARTESIAN_POINT ( 'NONE',  ( 186.7423748293213066, 36.79335956793068618, -19.00000000000003908 ) ) ;
#16434 = VERTEX_POINT ( 'NONE', #6348 ) ;
#16435 = LINE ( 'NONE', #11771, #16725 ) ;
#16436 = ORIENTED_EDGE ( 'NONE', *, *, #18769, .T. ) ;
#16437 = CARTESIAN_POINT ( 'NONE',  ( 229.4823745501375072, 36.26080457024635706, -13.97349461567483608 ) ) ;
#16438 = CARTESIAN_POINT ( 'NONE',  ( 192.7356731787757838, 6.693688996011149861, -17.08769543353810505 ) ) ;
#16439 = FACE_OUTER_BOUND ( 'NONE', #16742, .T. ) ;
#16440 = CLOSED_SHELL ( 'NONE', ( #18071, #12246, #17454, #4636, #12747, #12908, #6300, #6598, #12379, #13450, #1121, #13008, #14375, #5180, #7447, #19894, #11181, #10942, #2235, #481, #10491, #3061, #8363, #3673, #13532, #8741, #3651 ) ) ;
#16441 = ORIENTED_EDGE ( 'NONE', *, *, #14961, .F. ) ;
#16442 = CARTESIAN_POINT ( 'NONE',  ( 212.8872982515398178, 6.781229772587438198, -24.85758746085098991 ) ) ;
#16443 = LINE ( 'NONE', #8696, #11990 ) ;
#16444 = DIRECTION ( 'NONE',  ( 0.000000000000000000, 0.000000000000000000, 1.000000000000000000 ) ) ;
#16445 = ORIENTED_EDGE ( 'NONE', *, *, #5574, .F. ) ;
#16446 = CARTESIAN_POINT ( 'NONE',  ( 199.5603494194345444, -0.9130877231049959741, -19.34736286182874565 ) ) ;
#16447 = CARTESIAN_POINT ( 'NONE',  ( 191.0833833835253301, 36.99024094849632860, -9.087049258353282255 ) ) ;
#16448 = CARTESIAN_POINT ( 'NONE',  ( -15.99999999999991651, 71.61437827766162911, -4.999999999999997335 ) ) ;
#16449 = CARTESIAN_POINT ( 'NONE',  ( 75.55536774603304195, 52.69641891097137432, -16.70586935774736759 ) ) ;
#16451 = VERTEX_POINT ( 'NONE', #14346 ) ;
#16450 = ORIENTED_EDGE ( 'NONE', *, *, #7784, .F. ) ;
#16452 = ORIENTED_EDGE ( 'NONE', *, *, #11471, .F. ) ;
#16453 = AXIS2_PLACEMENT_3D ( 'NONE', #20732, #10559, #15467 ) ;
#16454 = VERTEX_POINT ( 'NONE', #15925 ) ;
#16455 = DIRECTION ( 'NONE',  ( -0.8660254037844358210, -0.5000000000000049960, 0.000000000000000000 ) ) ;
#16456 = ORIENTED_EDGE ( 'NONE', *, *, #2015, .T. ) ;
#16457 = VECTOR ( 'NONE', #3473, 1000.000000000000114 ) ;
#16458 = CARTESIAN_POINT ( 'NONE',  ( 10.40000000000000036, 0.000000000000000000, 0.000000000000000000 ) ) ;
#16459 = CIRCLE ( 'NONE', #6961, 1.000000000000000888 ) ;
#16460 = CARTESIAN_POINT ( 'NONE',  ( -19.61372346390630028, 79.99792423946925624, -12.24236967450913660 ) ) ;
#16461 = CARTESIAN_POINT ( 'NONE',  ( 219.1067971192485686, 36.72480411789796051, -17.14987233279964229 ) ) ;
#16462 = CARTESIAN_POINT ( 'NONE',  ( 5.000000000000004441, 2.342598717236899830, -4.057500000000030305 ) ) ;
#16463 = ORIENTED_EDGE ( 'NONE', *, *, #5717, .T. ) ;
#16464 = B_SPLINE_CURVE_WITH_KNOTS ( 'NONE', 3,
 ( #3190, #8152, #12641, #3289 ),
 .UNSPECIFIED., .F., .F.,
 ( 4, 4 ),
 ( 7.412987158413563422E-07, 0.0005862296544554486703 ),
 .UNSPECIFIED. ) ;
#16465 = DIRECTION ( 'NONE',  ( 0.000000000000000000, -0.5746640192525130919, 0.8183894335684859245 ) ) ;
#16466 = CARTESIAN_POINT ( 'NONE',  ( 80.37830472862586362, 65.70931303850179006, 0.4817205432224337947 ) ) ;
#16467 = EDGE_CURVE ( 'NONE', #2710, #4917, #4670, .T. ) ;
#16468 = CARTESIAN_POINT ( 'NONE',  ( 9.999999999999998224, 0.000000000000000000, 0.000000000000000000 ) ) ;
#16469 = VERTEX_POINT ( 'NONE', #4572 ) ;
#16470 = AXIS2_PLACEMENT_3D ( 'NONE', #4802, #11166, #16455 ) ;
#16471 = PLANE ( 'NONE',  #15916 ) ;
#16472 = DIRECTION ( 'NONE',  ( 0.7999999999999998224, 0.000000000000000000, -0.6000000000000000888 ) ) ;
#16473 = CIRCLE ( 'NONE', #19851, 7.960520131757803597 ) ;
#16474 = CYLINDRICAL_SURFACE ( 'NONE', #49, 15.00000000000000000 ) ;
#16476 = ORIENTED_EDGE ( 'NONE', *, *, #11982, .T. ) ;
#16475 = ORIENTED_EDGE ( 'NONE', *, *, #12360, .T. ) ;
#16477 = LINE ( 'NONE', #1960, #7493 ) ;
#16478 = LINE ( 'NONE', #11815, #4787 ) ;
#16479 = CARTESIAN_POINT ( 'NONE',  ( 227.5312376355471145, 39.64027283883993391, -14.00000000000005507 ) ) ;
#16480 = EDGE_CURVE ( 'NONE', #10313, #11034, #8000, .T. ) ;
#16481 = CARTESIAN_POINT ( 'NONE',  ( 81.47374219290158237, 55.54988310573300936, -22.87663793174895943 ) ) ;
#16482 = CARTESIAN_POINT ( 'NONE',  ( -27.93151244679091505, 6.473849509709803662, -3.824115908589273971 ) ) ;
#16483 = LINE ( 'NONE', #7722, #7585 ) ;
#16484 = ORIENTED_EDGE ( 'NONE', *, *, #10011, .F. ) ;
#16485 = VECTOR ( 'NONE', #18314, 1000.000000000000227 ) ;
#16486 = CARTESIAN_POINT ( 'NONE',  ( 62.64765726746416874, 74.40936579681903140, -21.49814275265928742 ) ) ;
#16487 = LINE ( 'NONE', #7351, #2357 ) ;
#16488 = EDGE_CURVE ( 'NONE', #12271, #8555, #18542, .T. ) ;
#16489 = ORIENTED_EDGE ( 'NONE', *, *, #19902, .T. ) ;
#16490 = ADVANCED_FACE ( 'NONE', ( #4772 ), #8942, .F. ) ;
#16491 = DIRECTION ( 'NONE',  ( 0.000000000000000000, 0.000000000000000000, -1.000000000000000000 ) ) ;
#16492 = CARTESIAN_POINT ( 'NONE',  ( -3.221035240742360362, 54.22335479770934086, -2.040458165079695796 ) ) ;
#16493 = CARTESIAN_POINT ( 'NONE',  ( -15.53444873921510272, 80.00000000000001421, -12.49812590152206404 ) ) ;
#16494 = DIRECTION ( 'NONE',  ( 0.000000000000000000, 6.938893903907177533E-18, 1.000000000000000000 ) ) ;
#16495 = FACE_OUTER_BOUND ( 'NONE', #8338, .T. ) ;
#16496 = CARTESIAN_POINT ( 'NONE',  ( 7.342598717236928252, 0.000000000000000000, 0.000000000000000000 ) ) ;
#16497 = B_SPLINE_CURVE_WITH_KNOTS ( 'NONE', 3,
 ( #17706, #17800, #9825, #9623 ),
 .UNSPECIFIED., .F., .F.,
 ( 4, 4 ),
 ( 8.322893307755415259E-06, 0.0004399335472996286221 ),
 .UNSPECIFIED. ) ;
#16499 = EDGE_LOOP ( 'NONE', ( #14842, #6094, #18646, #7149, #17185 ) ) ;
#16498 = VERTEX_POINT ( 'NONE', #11254 ) ;
#16500 = EDGE_LOOP ( 'NONE', ( #3247, #4854, #14177, #20485 ) ) ;
#16501 = DIRECTION ( 'NONE',  ( 0.5566703992264085965, 0.3213938048432680161, -0.7660444431189865622 ) ) ;
#16502 = CARTESIAN_POINT ( 'NONE',  ( 226.6211368133091923, 39.11482588413117867, -14.00000000000005507 ) ) ;
#16503 = VERTEX_POINT ( 'NONE', #17721 ) ;
#16504 = ORIENTED_EDGE ( 'NONE', *, *, #18192, .F. ) ;
#16505 = ADVANCED_FACE ( 'NONE', ( #9641 ), #1939, .T. ) ;
#16506 = ORIENTED_EDGE ( 'NONE', *, *, #19616, .F. ) ;
#16507 = AXIS2_PLACEMENT_3D ( 'NONE', #12382, #17563, #1030 ) ;
#16508 = CARTESIAN_POINT ( 'NONE',  ( -16.18042569387133511, 58.38562172233856984, -4.999999999999989342 ) ) ;
#16509 = PRODUCT ( 'Part5^MAS-328', 'Part5^MAS-328', '', ( #2574 ) ) ;
#16510 = CARTESIAN_POINT ( 'NONE',  ( 228.7555033867736540, 38.49924824681247060, -10.80501622924634475 ) ) ;
#16511 = DIRECTION ( 'NONE',  ( -0.5000000000000051070, 0.8660254037844359321, -0.000000000000000000 ) ) ;
#16512 = VERTEX_POINT ( 'NONE', #10526 ) ;
#16513 = CIRCLE ( 'NONE', #10746, 5.400000000000001243 ) ;
#16514 = CARTESIAN_POINT ( 'NONE',  ( 0.000000000000000000, -10.00000000000000000, 0.000000000000000000 ) ) ;
#16515 = CARTESIAN_POINT ( 'NONE',  ( 25.17200000000003612, 0.000000000000000000, 5.000000000000000888 ) ) ;
#16516 = EDGE_CURVE ( 'NONE', #270, #12839, #7599, .T. ) ;
#16517 = ORIENTED_EDGE ( 'NONE', *, *, #210, .F. ) ;
#16518 = FACE_OUTER_BOUND ( 'NONE', #9511, .T. ) ;
#16519 = EDGE_CURVE ( 'NONE', #16924, #17685, #19809, .T. ) ;
#16520 = PRESENTATION_LAYER_ASSIGNMENT (  '', '', ( #13819 ) ) ;
#16521 = DIRECTION ( 'NONE',  ( -0.5000000000000051070, 0.8660254037844359321, -0.000000000000000000 ) ) ;
#16522 = CARTESIAN_POINT ( 'NONE',  ( -28.94626959558488011, 56.84162378296022666, 0.1050044003684389854 ) ) ;
#16523 = CARTESIAN_POINT ( 'NONE',  ( -16.32953223445319679, 20.09941697557067997, 12.50000000000000178 ) ) ;
#16524 = AXIS2_PLACEMENT_3D ( 'NONE', #19744, #8190, #11486 ) ;
#16525 = CARTESIAN_POINT ( 'NONE',  ( 229.3736054848727690, 37.42866400863998422, -11.75146085096538862 ) ) ;
#16526 =( BOUNDED_SURFACE ( )  B_SPLINE_SURFACE ( 3, 2, ( 
 ( #13897, #4248, #13796 ),
 ( #12202, #16864, #2345 ),
 ( #8803, #9103, #8695 ),
 ( #15302, #18775, #20143 ),
 ( #5606, #10699, #19927 ),
 ( #12094, #5394, #20245 ),
 ( #18563, #18351, #4143 ),
 ( #10481, #17081, #16758 ),
 ( #7307, #2240, #2453 ),
 ( #15404, #2560, #9005 ),
 ( #16024, #7730, #20456 ),
 ( #15715, #19289, #20862 ),
 ( #6336, #20558, #6136 ),
 ( #1486, #4759, #2769 ),
 ( #3176, #10803, #17283 ),
 ( #11241, #1285, #15911 ) ),
 .UNSPECIFIED., .F., .F., .T. ) 
 B_SPLINE_SURFACE_WITH_KNOTS ( ( 4, 2, 2, 2, 2, 2, 2, 4 ),
 ( 3, 3 ),
 ( 0.09394529277310080528, 0.09803747693844724886, 0.1000835690211204776, 0.1011066150624570781, 0.1021296611037936924, 0.1062218452691401360, 0.1082679373518133648, 0.1103140294344865796 ),
 ( 0.000000000000000000, 1.000000000000000000 ),
 .UNSPECIFIED. ) 
 GEOMETRIC_REPRESENTATION_ITEM ( )  RATIONAL_B_SPLINE_SURFACE ( (
 ( 1.000000000000000000, 0.7167790485004653656, 1.000000000000000000),
 ( 1.000000000000000000, 0.7312157917998166612, 1.000000000000000000),
 ( 1.000000000000000000, 0.7466500244729707969, 1.000000000000000000),
 ( 1.000000000000000000, 0.7689011243010751562, 1.000000000000000000),
 ( 1.000000000000000000, 0.7761748643738399789, 1.000000000000000000),
 ( 1.000000000000000000, 0.7866334538989935288, 1.000000000000000000),
 ( 1.000000000000000000, 0.7900487569768197549, 1.000000000000000000),
 ( 1.000000000000000000, 0.7966228133242926335, 1.000000000000000000),
 ( 1.000000000000000000, 0.7997907721098268530, 1.000000000000000000),
 ( 1.000000000000000000, 0.8149753752735824364, 1.000000000000000000),
 ( 1.000000000000000000, 0.8250225257833745385, 1.000000000000000000),
 ( 1.000000000000000000, 0.8359195949012849791, 1.000000000000000000),
 ( 1.000000000000000000, 0.8388534816487658308, 1.000000000000000000),
 ( 1.000000000000000000, 0.8430760250471756034, 1.000000000000000000),
 ( 1.000000000000000000, 0.8443918141125164034, 1.000000000000000000),
 ( 1.000000000000000000, 0.8449065510952332714, 1.000000000000000000) ) ) 
 REPRESENTATION_ITEM ( '' )  SURFACE ( )  );
#16527 = VERTEX_POINT ( 'NONE', #19596 ) ;
#16528 = CARTESIAN_POINT ( 'NONE',  ( 59.60168565680741892, 84.71166588009855047, -8.872864206773611429 ) ) ;
#16529 = EDGE_CURVE ( 'NONE', #13343, #2929, #4964, .T. ) ;
#16530 = ORIENTED_EDGE ( 'NONE', *, *, #6831, .T. ) ;
#16531 = EDGE_CURVE ( 'NONE', #139, #2303, #14502, .T. ) ;
#16532 = ORIENTED_EDGE ( 'NONE', *, *, #6302, .T. ) ;
#16533 = CARTESIAN_POINT ( 'NONE',  ( 208.5538622303137686, 11.70232678560638462, -2.669358488461177625 ) ) ;
#16534 = CARTESIAN_POINT ( 'NONE',  ( 225.6488786369508830, 42.90061426249287990, -15.02729838650890493 ) ) ;
#16535 = AXIS2_PLACEMENT_3D ( 'NONE', #2578, #13916, #14029 ) ;
#16536 = VERTEX_POINT ( 'NONE', #215 ) ;
#16537 = FACE_OUTER_BOUND ( 'NONE', #9702, .T. ) ;
#16538 = ORIENTED_EDGE ( 'NONE', *, *, #20645, .T. ) ;
#16539 = ITEM_DEFINED_TRANSFORMATION ( 'NONE', 'NONE', #1985,  #18233 ) ;
#16540 = EDGE_CURVE ( 'NONE', #1594, #10851, #9838, .T. ) ;
#16541 = CARTESIAN_POINT ( 'NONE',  ( -29.34053455105015829, 65.74999999999997158, 3.134647201270610140 ) ) ;
#16542 = VERTEX_POINT ( 'NONE', #3288 ) ;
#16543 = CARTESIAN_POINT ( 'NONE',  ( 198.1209940990830205, -1.744099904769494280, -9.448537646917499089 ) ) ;
#16544 = DIRECTION ( 'NONE',  ( 0.5000000000000054401, -0.8660254037844354880, 0.000000000000000000 ) ) ;
#16545 = PLANE ( 'NONE',  #19383 ) ;
#16546 = EDGE_CURVE ( 'NONE', #4987, #7633, #5176, .T. ) ;
#16547 = ORIENTED_EDGE ( 'NONE', *, *, #12757, .F. ) ;
#16548 = CARTESIAN_POINT ( 'NONE',  ( 229.7718384214206822, 36.73890432929155736, -11.78784277354609422 ) ) ;
#16549 = FACE_OUTER_BOUND ( 'NONE', #10302, .T. ) ;
#16550 = CARTESIAN_POINT ( 'NONE',  ( 215.8997106868019387, 9.293266993639628382, -23.06309126349817618 ) ) ;
#16551 = AXIS2_PLACEMENT_3D ( 'NONE', #18699, #9037, #2595 ) ;
#16552 = ORIENTED_EDGE ( 'NONE', *, *, #18315, .T. ) ;
#16553 = CARTESIAN_POINT ( 'NONE',  ( 5.000000000000000000, 4.685197434473812983, -6.938893903907228378E-15 ) ) ;
#16554 = EDGE_CURVE ( 'NONE', #18950, #1221, #6762, .T. ) ;
#16556 = CYLINDRICAL_SURFACE ( 'NONE', #1399, 12.47473710546057646 ) ;
#16555 = PRODUCT_DEFINITION_FORMATION_WITH_SPECIFIED_SOURCE ( 'ANY', '', #18380, .NOT_KNOWN. ) ;
#16557 = CARTESIAN_POINT ( 'NONE',  ( -12.00682109638796291, 68.17699921526258322, -3.011576861204072753 ) ) ;
#16558 = CARTESIAN_POINT ( 'NONE',  ( 78.13892160451581503, 52.41879779276553819, -15.80834409985953926 ) ) ;
#16560 = VERTEX_POINT ( 'NONE', #1808 ) ;
#16559 = ORIENTED_EDGE ( 'NONE', *, *, #5764, .T. ) ;
#16561 = EDGE_CURVE ( 'NONE', #15958, #270, #13361, .T. ) ;
#16562 = ORIENTED_EDGE ( 'NONE', *, *, #8821, .F. ) ;
#16563 = CARTESIAN_POINT ( 'NONE',  ( 26.00000000000000355, 0.000000000000000000, 0.000000000000000000 ) ) ;
#16564 = AXIS2_PLACEMENT_3D ( 'NONE', #8668, #5362, #18318 ) ;
#16565 = ORIENTED_EDGE ( 'NONE', *, *, #3336, .T. ) ;
#16566 = DIRECTION ( 'NONE',  ( 0.5000000000000057732, -0.8660254037844353769, 0.000000000000000000 ) ) ;
#16567 = CARTESIAN_POINT ( 'NONE',  ( -19.56641610727023561, 79.99999999999583622, -11.99131545410286925 ) ) ;
#16568 = CARTESIAN_POINT ( 'NONE',  ( 221.7111930334534406, 32.18635333779653962, -14.35673080489372744 ) ) ;
#16569 = CARTESIAN_POINT ( 'NONE',  ( 205.3906008270068071, 3.225829587143459243, -2.044871543906942701 ) ) ;
#16570 = VERTEX_POINT ( 'NONE', #317 ) ;
#16571 = LINE ( 'NONE', #13504, #20712 ) ;
#16572 = VECTOR ( 'NONE', #4492, 1000.000000000000000 ) ;
#16573 = CARTESIAN_POINT ( 'NONE',  ( 57.68399219382784793, 76.53693708094122883, -18.53323648005439139 ) ) ;
#16574 = CARTESIAN_POINT ( 'NONE',  ( 5.000000000000000000, 7.027796151710712813, -4.057500000000007212 ) ) ;
#16575 = ORIENTED_EDGE ( 'NONE', *, *, #8792, .T. ) ;
#16576 = LINE ( 'NONE', #6698, #19637 ) ;
#16577 = DIRECTION ( 'NONE',  ( 0.5000000000000045519, -0.8660254037844361541, 0.000000000000000000 ) ) ;
#16578 = DIRECTION ( 'NONE',  ( 0.000000000000000000, 0.000000000000000000, -1.000000000000000000 ) ) ;
#16579 = CARTESIAN_POINT ( 'NONE',  ( -13.42396981071245854, 80.00000000000414957, -12.24234612424543478 ) ) ;
#16580 = ORIENTED_EDGE ( 'NONE', *, *, #7406, .F. ) ;
#16581 = AXIS2_PLACEMENT_3D ( 'NONE', #8748, #4088, #5555 ) ;
#16582 = CARTESIAN_POINT ( 'NONE',  ( 227.5238769672030514, 40.63248778145290174, -9.834987871251030356 ) ) ;
#16583 = LINE ( 'NONE', #9985, #16977 ) ;
#16584 = FACE_OUTER_BOUND ( 'NONE', #1774, .T. ) ;
#16585 = CARTESIAN_POINT ( 'NONE',  ( 194.8942117681098125, 18.53182819120163671, -14.00000000000005507 ) ) ;
#16586 = EDGE_CURVE ( 'NONE', #13549, #38, #15078, .T. ) ;
#16587 = CARTESIAN_POINT ( 'NONE',  ( -28.49991287530916040, 6.470303912909706412, -0.3949351193324712184 ) ) ;
#16588 = CARTESIAN_POINT ( 'NONE',  ( 203.0627220339503936, 1.881828139331499727, -24.79563718815128226 ) ) ;
#16589 = ORIENTED_EDGE ( 'NONE', *, *, #11493, .T. ) ;
#16590 = CARTESIAN_POINT ( 'NONE',  ( 82.31356959450070576, 63.34177109540507189, -25.39725247914766726 ) ) ;
#16591 = AXIS2_PLACEMENT_3D ( 'NONE', #672, #10621, #4055 ) ;
#16592 = CARTESIAN_POINT ( 'NONE',  ( -6.481806088851808312, 45.01191145235649316, -8.139083654344593910 ) ) ;
#16593 = VECTOR ( 'NONE', #6290, 1000.000000000000114 ) ;
#16594 = ORIENTED_EDGE ( 'NONE', *, *, #6008, .T. ) ;
#16595 = CARTESIAN_POINT ( 'NONE',  ( 201.9876788769632299, 25.95811253888945203, -15.19853025469339869 ) ) ;
#16596 = CARTESIAN_POINT ( 'NONE',  ( -3.688831311464842777, 52.40708535496389686, 2.175092931272005981 ) ) ;
#16597 = CARTESIAN_POINT ( 'NONE',  ( 212.7427532632225962, 7.470596775315875071, -25.46066938576263894 ) ) ;
#16598 = DIRECTION ( 'NONE',  ( 0.6299240516454601702, 0.3636868207865310287, 0.6862416378687270502 ) ) ;
#16599 = CARTESIAN_POINT ( 'NONE',  ( 98.91428619100412334, 200.0914894846854679, 8.500000000000049738 ) ) ;
#16600 = EDGE_CURVE ( 'NONE', #10224, #13939, #5074, .T. ) ;
#16601 = DIRECTION ( 'NONE',  ( -0.1017280065263260758, 0.1761980758562863847, 0.9790840876823205807 ) ) ;
#16603 = VERTEX_POINT ( 'NONE', #1700 ) ;
#16602 = ORIENTED_EDGE ( 'NONE', *, *, #5219, .F. ) ;
#16604 = ORIENTED_EDGE ( 'NONE', *, *, #10562, .F. ) ;
#16605 = CARTESIAN_POINT ( 'NONE',  ( 218.5362608324210782, 10.04265983930142347, -9.928836400542515150 ) ) ;
#16606 = VECTOR ( 'NONE', #2532, 1000.000000000000227 ) ;
#16607 = FACE_OUTER_BOUND ( 'NONE', #5740, .T. ) ;
#16608 = ORIENTED_EDGE ( 'NONE', *, *, #3697, .F. ) ;
#16609 = ORIENTED_EDGE ( 'NONE', *, *, #1587, .F. ) ;
#16610 = ORIENTED_EDGE ( 'NONE', *, *, #7974, .F. ) ;
#16611 = CARTESIAN_POINT ( 'NONE',  ( 193.6293134455680445, 7.209632444602317669, -12.64773574313024085 ) ) ;
#16612 = VECTOR ( 'NONE', #12603, 1000.000000000000114 ) ;
#16613 = CARTESIAN_POINT ( 'NONE',  ( 197.0442994948038233, 5.057277642004744500, -20.52105855319921091 ) ) ;
#16614 = EDGE_LOOP ( 'NONE', ( #20869, #15203, #56, #5614 ) ) ;
#16615 = EDGE_CURVE ( 'NONE', #12912, #6578, #11063, .T. ) ;
#16616 = VECTOR ( 'NONE', #11415, 1000.000000000000227 ) ;
#16617 = CARTESIAN_POINT ( 'NONE',  ( 201.7640869814541134, 0.3592407515502875626, -5.407152407593845744 ) ) ;
#16618 = ADVANCED_FACE ( 'NONE', ( #8254, #11770 ), #18027, .T. ) ;
#16619 = CYLINDRICAL_SURFACE ( 'NONE', #18538, 4.999999999999989342 ) ;
#16620 = AXIS2_PLACEMENT_3D ( 'NONE', #12711, #4439, #15796 ) ;
#16621 = EDGE_LOOP ( 'NONE', ( #4946, #4546, #13940, #6795, #10356 ) ) ;
#16622 = CIRCLE ( 'NONE', #3405, 5.000000000000002665 ) ;
#16623 = DIRECTION ( 'NONE',  ( -0.5000000000000044409, 0.8660254037844360431, 4.006172263299080068E-16 ) ) ;
#16624 = CARTESIAN_POINT ( 'NONE',  ( -27.91715957486725230, 46.29657224408730798, -3.824975988489407897 ) ) ;
#16625 = DIRECTION ( 'NONE',  ( -0.4999999999999995004, 0.8660254037844390407, 0.000000000000000000 ) ) ;
#16626 = AXIS2_PLACEMENT_3D ( 'NONE', #13437, #11738, #5247 ) ;
#16627 = ORIENTED_EDGE ( 'NONE', *, *, #15511, .F. ) ;
#16628 = PLANE ( 'NONE',  #14572 ) ;
#16629 = AXIS2_PLACEMENT_3D ( 'NONE', #787, #13827, #5537 ) ;
#16630 = DIRECTION ( 'NONE',  ( 0.8660254037844380415, 0.5000000000000014433, 0.000000000000000000 ) ) ;
#16632 = ORIENTED_EDGE ( 'NONE', *, *, #2566, .F. ) ;
#16631 = ORIENTED_EDGE ( 'NONE', *, *, #7593, .F. ) ;
#16633 = ORIENTED_EDGE ( 'NONE', *, *, #1132, .T. ) ;
#16634 = CARTESIAN_POINT ( 'NONE',  ( 54.51375964220392234, 77.88617331000196486, -14.23577307808955972 ) ) ;
#16635 = ORIENTED_EDGE ( 'NONE', *, *, #6909, .F. ) ;
#16636 = ORIENTED_EDGE ( 'NONE', *, *, #16792, .T. ) ;
#16637 = ORIENTED_EDGE ( 'NONE', *, *, #6523, .F. ) ;
#16638 = FACE_OUTER_BOUND ( 'NONE', #11008, .T. ) ;
#16639 = CARTESIAN_POINT ( 'NONE',  ( 194.2655634166889342, 7.576971536700876086, -21.18305361806748977 ) ) ;
#16640 = ADVANCED_FACE ( 'NONE', ( #16537 ), #10369, .T. ) ;
#16641 = AXIS2_PLACEMENT_3D ( 'NONE', #12162, #1238, #18625 ) ;
#16642 = CARTESIAN_POINT ( 'NONE',  ( 67.36131599811847082, 207.2831476774790644, 11.00000000000001066 ) ) ;
#16643 = EDGE_LOOP ( 'NONE', ( #12673, #2186 ) ) ;
#16644 = VECTOR ( 'NONE', #10163, 999.9999999999998863 ) ;
#16645 = CIRCLE ( 'NONE', #15323, 7.155882939242646401 ) ;
#16646 = VECTOR ( 'NONE', #16019, 1000.000000000000000 ) ;
#16647 = CARTESIAN_POINT ( 'NONE',  ( 214.2742449478047604, 15.00499128741754262, -7.425127016398544555 ) ) ;
#16648 = VERTEX_POINT ( 'NONE', #11347 ) ;
#16649 = CARTESIAN_POINT ( 'NONE',  ( 35.35427444295658717, 182.7209698509878422, 11.00000000000001243 ) ) ;
#16650 = CARTESIAN_POINT ( 'NONE',  ( 208.1960812450810465, 4.072754371081482638, -0.8632678296711639998 ) ) ;
#16651 = EDGE_CURVE ( 'NONE', #16570, #19425, #2129, .T. ) ;
#16652 = CARTESIAN_POINT ( 'NONE',  ( 1.484819526751607999, 80.00000000000000000, 0.7287565553229443660 ) ) ;
#16653 = DIRECTION ( 'NONE',  ( 0.000000000000000000, 0.000000000000000000, -1.000000000000000000 ) ) ;
#16654 = FACE_OUTER_BOUND ( 'NONE', #1386, .T. ) ;
#16655 = B_SPLINE_CURVE_WITH_KNOTS ( 'NONE', 3,
 ( #5624, #980, #13813, #12440 ),
 .UNSPECIFIED., .F., .F.,
 ( 4, 4 ),
 ( 4.671652097665054242E-07, 0.0005663933875071499539 ),
 .UNSPECIFIED. ) ;
#16656 = ORIENTED_EDGE ( 'NONE', *, *, #18498, .F. ) ;
#16657 = DIRECTION ( 'NONE',  ( -0.8660254037844357100, -0.5000000000000051070, 0.000000000000000000 ) ) ;
#16658 = PRESENTATION_LAYER_ASSIGNMENT (  '', '', ( #11923 ) ) ;
#16659 = CARTESIAN_POINT ( 'NONE',  ( 230.0820949324995297, 36.20152428872393102, -13.99751724578390721 ) ) ;
#16660 = FACE_OUTER_BOUND ( 'NONE', #17037, .T. ) ;
#16661 = ORIENTED_EDGE ( 'NONE', *, *, #12775, .F. ) ;
#16662 = CONICAL_SURFACE ( 'NONE', #15994, 4.999999999999995559, 1.029744258676653867 ) ;
#16664 = EDGE_CURVE ( 'NONE', #16030, #5457, #3957, .T. ) ;
#16663 = CARTESIAN_POINT ( 'NONE',  ( 81.55608559449183304, 62.10651918161714491, 0.1764946495667281956 ) ) ;
#16665 = CARTESIAN_POINT ( 'NONE',  ( -13.09058959453371074, 70.37881519986052581, -4.068652614656581790 ) ) ;
#16666 = CARTESIAN_POINT ( 'NONE',  ( 79.86683865086524747, 50.89072876157985803, -6.984412221717008151 ) ) ;
#16667 = EDGE_CURVE ( 'NONE', #17532, #16536, #13475, .T. ) ;
#16669 = EDGE_LOOP ( 'NONE', ( #18050, #14245, #6576 ) ) ;
#16668 = ORIENTED_EDGE ( 'NONE', *, *, #13837, .T. ) ;
#16670 = ORIENTED_EDGE ( 'NONE', *, *, #20809, .T. ) ;
#16671 = FACE_OUTER_BOUND ( 'NONE', #8600, .T. ) ;
#16672 = VERTEX_POINT ( 'NONE', #19705 ) ;
#16673 = CARTESIAN_POINT ( 'NONE',  ( 75.15809445383052889, 52.16896057810638609, -10.30453221435095834 ) ) ;
#16674 = CARTESIAN_POINT ( 'NONE',  ( -17.30218132643816276, 79.99997331865614569, -12.46740305798945592 ) ) ;
#16675 = AXIS2_PLACEMENT_3D ( 'NONE', #14145, #12542, #9331 ) ;
#16676 = CARTESIAN_POINT ( 'NONE',  ( 219.1067971192485686, 36.72480411789796051, -17.14987233279964229 ) ) ;
#16677 = CARTESIAN_POINT ( 'NONE',  ( 218.4555304624101097, 38.05874925762264382, -15.87804042560534512 ) ) ;
#16678 = EDGE_CURVE ( 'NONE', #1138, #16010, #4644, .T. ) ;
#16679 = ORIENTED_EDGE ( 'NONE', *, *, #19027, .F. ) ;
#16680 = AXIS2_PLACEMENT_3D ( 'NONE', #16395, #13753, #13440 ) ;
#16681 = ADVANCED_FACE ( 'NONE', ( #12308 ), #9095, .F. ) ;
#16682 = PLANE ( 'NONE',  #9872 ) ;
#16683 = DIRECTION ( 'NONE',  ( 0.2597919750177127840, -0.4499729001293399921, 0.8544194045464951204 ) ) ;
#16684 = CARTESIAN_POINT ( 'NONE',  ( 214.9458835816058979, 7.969754567050957306, -23.47937149798938350 ) ) ;
#16685 = VERTEX_POINT ( 'NONE', #16746 ) ;
#16687 = EDGE_CURVE ( 'NONE', #6628, #4158, #18873, .T. ) ;
#16686 = DIRECTION ( 'NONE',  ( -0.6299240516454601702, -0.3636868207865310287, -0.6862416378687270502 ) ) ;
#16688 = CARTESIAN_POINT ( 'NONE',  ( 16.51452848080062097, 235.3523670591319217, -13.99999999999994493 ) ) ;
#16689 = B_SPLINE_CURVE_WITH_KNOTS ( 'NONE', 3,
 ( #14160, #20592, #5857, #18914 ),
 .UNSPECIFIED., .F., .F.,
 ( 4, 4 ),
 ( 5.955297919916776097E-07, 0.0004526487715719124203 ),
 .UNSPECIFIED. ) ;
#16690 = B_SPLINE_CURVE_WITH_KNOTS ( 'NONE', 3,
 ( #14173, #12574, #11286, #19037 ),
 .UNSPECIFIED., .F., .F.,
 ( 4, 4 ),
 ( 5.849083921015304242E-06, 0.0005717753062168848092 ),
 .UNSPECIFIED. ) ;
#16691 = CYLINDRICAL_SURFACE ( 'NONE', #8171, 3.902363844300889451 ) ;
#16692 = CARTESIAN_POINT ( 'NONE',  ( -0.4956845319646441261, 78.79719334215242554, -6.605250029488230368 ) ) ;
#16693 = AXIS2_PLACEMENT_3D ( 'NONE', #11125, #14227, #17598 ) ;
#16695 = ORIENTED_EDGE ( 'NONE', *, *, #2650, .F. ) ;
#16694 = ORIENTED_EDGE ( 'NONE', *, *, #16091, .T. ) ;
#16696 = CARTESIAN_POINT ( 'NONE',  ( 209.5488276859553594, 16.40076827665816239, -25.36561010639692881 ) ) ;
#16697 = CARTESIAN_POINT ( 'NONE',  ( 219.8041001712509512, 35.51703980355691215, -10.43865930680574827 ) ) ;
#16698 = DIRECTION ( 'NONE',  ( -0.8660254037844378194, -0.5000000000000013323, -0.000000000000000000 ) ) ;
#16699 = EDGE_CURVE ( 'NONE', #18617, #17439, #4131, .T. ) ;
#16700 = CARTESIAN_POINT ( 'NONE',  ( 80.07168963752003776, 51.46048616005985821, -18.93354426913304422 ) ) ;
#16701 = CARTESIAN_POINT ( 'NONE',  ( -29.99999999999999645, 5.000000000000000000, 8.929304381912043453 ) ) ;
#16702 =( LENGTH_UNIT ( ) NAMED_UNIT ( * ) SI_UNIT ( .MILLI., .METRE. ) );
#16703 = DIRECTION ( 'NONE',  ( -0.8660254037844360431, -0.5000000000000044409, 5.976026924694052093E-17 ) ) ;
#16704 = ORIENTED_EDGE ( 'NONE', *, *, #13807, .F. ) ;
#16705 = CARTESIAN_POINT ( 'NONE',  ( 82.20437289446037710, 57.97282872583890168, -24.17078908960660755 ) ) ;
#16706 = CARTESIAN_POINT ( 'NONE',  ( -8.767231887450829930, 45.07424775628126667, -10.22364500895912798 ) ) ;
#16707 = VECTOR ( 'NONE', #11410, 1000.000000000000000 ) ;
#16708 = EDGE_LOOP ( 'NONE', ( #12577, #7196 ) ) ;
#16709 = DIRECTION ( 'NONE',  ( 0.8660254037844361541, 0.5000000000000043299, 3.166650901095681677E-16 ) ) ;
#16710 = CARTESIAN_POINT ( 'NONE',  ( -3.063870802415169070, 57.44566917294824293, 0.4923802658666992516 ) ) ;
#16711 = CARTESIAN_POINT ( 'NONE',  ( -1.372481614566710251, 79.12694522062832903, -7.447838812965425603 ) ) ;
#16712 = CARTESIAN_POINT ( 'NONE',  ( 213.3216307924363946, 4.537449897911132624, -14.00000000000005507 ) ) ;
#16713 = FACE_OUTER_BOUND ( 'NONE', #10413, .T. ) ;
#16714 = DIRECTION ( 'NONE',  ( -0.8660254037844378194, -0.5000000000000013323, -0.000000000000000000 ) ) ;
#16716 = ORIENTED_EDGE ( 'NONE', *, *, #8472, .F. ) ;
#16715 = ORIENTED_EDGE ( 'NONE', *, *, #19091, .F. ) ;
#16717 = ORIENTED_EDGE ( 'NONE', *, *, #13583, .T. ) ;
#16718 = DIRECTION ( 'NONE',  ( -0.4895420438411626773, 0.8479116923739991041, -0.2034560130526446298 ) ) ;
#16719 = FACE_OUTER_BOUND ( 'NONE', #2429, .T. ) ;
#16720 = ORIENTED_EDGE ( 'NONE', *, *, #5295, .F. ) ;
#16721 = ORIENTED_EDGE ( 'NONE', *, *, #9668, .F. ) ;
#16722 = CARTESIAN_POINT ( 'NONE',  ( 81.33476212519650517, 64.63473428484439864, 0.4964296018791880538 ) ) ;
#16723 = CARTESIAN_POINT ( 'NONE',  ( 229.3261223513948721, 36.53144131726288890, -12.46964089162990064 ) ) ;
#16724 = DIRECTION ( 'NONE',  ( -0.8660254037844368202, -0.5000000000000032196, 0.000000000000000000 ) ) ;
#16725 = VECTOR ( 'NONE', #1918, 1000.000000000000000 ) ;
#16726 = AXIS2_PLACEMENT_3D ( 'NONE', #11128, #3177, #2976 ) ;
#16727 = ORIENTED_EDGE ( 'NONE', *, *, #8125, .F. ) ;
#16728 = DIRECTION ( 'NONE',  ( 6.608470384673549052E-16, -1.000000000000000000, 0.000000000000000000 ) ) ;
#16729 = CARTESIAN_POINT ( 'NONE',  ( -15.99999999999991651, 71.61437827766162911, -4.999999999999997335 ) ) ;
#16730 = DIRECTION ( 'NONE',  ( -0.8660254037844362651, -0.5000000000000042188, 6.872020471724002955E-17 ) ) ;
#16731 = CARTESIAN_POINT ( 'NONE',  ( -15.99999999999999289, 80.00000000000000000, 0.000000000000000000 ) ) ;
#16732 = CARTESIAN_POINT ( 'NONE',  ( -26.65066008881222359, 45.27454425555390571, -6.552074931230112753 ) ) ;
#16733 = CARTESIAN_POINT ( 'NONE',  ( 199.0679134205424816, -0.6821895407469270589, -8.485309299592096011 ) ) ;
#16734 = CIRCLE ( 'NONE', #8256, 5.000000000000000000 ) ;
#16735 = DIRECTION ( 'NONE',  ( 0.8660254037844360431, 0.5000000000000044409, -5.976026924694053325E-17 ) ) ;
#16736 = PLANE ( 'NONE',  #8667 ) ;
#16737 = ADVANCED_FACE ( 'NONE', ( #20339 ), #4018, .F. ) ;
#16739 = VERTEX_POINT ( 'NONE', #2548 ) ;
#16738 = ORIENTED_EDGE ( 'NONE', *, *, #6930, .T. ) ;
#16740 = CARTESIAN_POINT ( 'NONE',  ( 60.40852599701213421, 84.09099035223172791, -17.30637792422236032 ) ) ;
#16741 = EDGE_LOOP ( 'NONE', ( #704, #17145, #16979, #13075, #9431, #13966 ) ) ;
#16742 = EDGE_LOOP ( 'NONE', ( #7083, #11278, #11792, #5541 ) ) ;
#16743 = DIRECTION ( 'NONE',  ( 1.000000000000000000, 0.000000000000000000, 0.000000000000000000 ) ) ;
#16744 = LINE ( 'NONE', #8889, #19822 ) ;
#16745 = EDGE_LOOP ( 'NONE', ( #11491, #479, #20259, #3106 ) ) ;
#16746 = CARTESIAN_POINT ( 'NONE',  ( 227.9152326730940672, 38.97517392395430846, -10.17395310825082611 ) ) ;
#16747 = VECTOR ( 'NONE', #19738, 1000.000000000000114 ) ;
#16748 = EDGE_CURVE ( 'NONE', #11548, #17011, #15394, .T. ) ;
#16749 = CARTESIAN_POINT ( 'NONE',  ( 10.49211908931699178, 5.000000000000000000, -5.000000000000000000 ) ) ;
#16750 = ORIENTED_EDGE ( 'NONE', *, *, #14148, .T. ) ;
#16751 = DIRECTION ( 'NONE',  ( 0.5000000000000045519, -0.8660254037844361541, -0.000000000000000000 ) ) ;
#16752 = DIRECTION ( 'NONE',  ( -1.000000000000000000, -0.000000000000000000, -0.000000000000000000 ) ) ;
#16753 = LINE ( 'NONE', #8902, #11914 ) ;
#16754 = CARTESIAN_POINT ( 'NONE',  ( 205.8264633344831225, 9.596613037118636669, -14.00000000000005507 ) ) ;
#16755 = CARTESIAN_POINT ( 'NONE',  ( 207.5960625376490043, 10.79531429386019958, -26.12540443289073977 ) ) ;
#16756 = ADVANCED_FACE ( 'NONE', ( #20030 ), #18442, .F. ) ;
#16757 = ORIENTED_EDGE ( 'NONE', *, *, #2821, .F. ) ;
#16758 = CARTESIAN_POINT ( 'NONE',  ( -32.68029730050665194, 71.85025536417415992, 0.8468720397201384698 ) ) ;
#16759 = CARTESIAN_POINT ( 'NONE',  ( 208.4761278624580711, 5.007259451653140125, -14.00000000000005507 ) ) ;
#16760 = DIRECTION ( 'NONE',  ( 0.5000000000000054401, -0.8660254037844354880, 0.000000000000000000 ) ) ;
#16761 = EDGE_CURVE ( 'NONE', #13251, #9080, #8919, .T. ) ;
#16762 = ORIENTED_EDGE ( 'NONE', *, *, #9126, .F. ) ;
#16763 = CARTESIAN_POINT ( 'NONE',  ( 81.10655718899693056, 54.43739570253208626, -2.927339837274431922 ) ) ;
#16764 = VERTEX_POINT ( 'NONE', #747 ) ;
#16765 = CARTESIAN_POINT ( 'NONE',  ( 199.6382066537783260, 23.53622389300110385, -14.00000000000005507 ) ) ;
#16766 = PLANE ( 'NONE',  #12717 ) ;
#16768 = EDGE_LOOP ( 'NONE', ( #19177, #17638, #8264, #9456, #20495, #12461 ) ) ;
#16767 = ORIENTED_EDGE ( 'NONE', *, *, #9637, .F. ) ;
#16769 = ADVANCED_FACE ( 'NONE', ( #952 ), #2227, .F. ) ;
#16770 = PRODUCT_CONTEXT ( 'NONE', #20813, 'mechanical' ) ;
#16771 = APPLICATION_CONTEXT ( 'automotive_design' ) ;
#16772 = DIRECTION ( 'NONE',  ( 0.000000000000000000, 0.000000000000000000, -1.000000000000000000 ) ) ;
#16773 = ORIENTED_EDGE ( 'NONE', *, *, #16748, .F. ) ;
#16774 = CARTESIAN_POINT ( 'NONE',  ( 209.8909370991932519, 2.556737970610027499, -14.00000000000005507 ) ) ;
#16775 = CLOSED_SHELL ( 'NONE', ( #19580, #17658, #11991, #19003, #10523, #1012, #443, #17387, #9333, #19606, #102, #2386, #15527, #18076, #17612, #10309, #18987, #19131, #15205, #5503, #13678, #10407, #18532, #1496, #8866, #15395, #6819, #7699 ) ) ;
#16776 = CARTESIAN_POINT ( 'NONE',  ( 216.6737232845935068, 8.967323284687328311, -21.59012016402729728 ) ) ;
#16777 = CARTESIAN_POINT ( 'NONE',  ( 201.5545410371157118, 7.661266810568780450, -3.125199447383423035 ) ) ;
#16778 = CARTESIAN_POINT ( 'NONE',  ( 227.5647218214154464, 40.56174241872900410, -17.53429396590401623 ) ) ;
#16779 = EDGE_CURVE ( 'NONE', #13470, #1032, #5593, .T. ) ;
#16780 = VERTEX_POINT ( 'NONE', #2439 ) ;
#16781 = VECTOR ( 'NONE', #12112, 1000.000000000000227 ) ;
#16782 = CARTESIAN_POINT ( 'NONE',  ( 210.6201421056092897, 5.472286561439484665, -25.76107385416583639 ) ) ;
#16783 = EDGE_CURVE ( 'NONE', #12266, #17006, #3292, .T. ) ;
#16784 = DIRECTION ( 'NONE',  ( 0.9949159024423646080, 0.000000000000000000, -0.1007092203688184640 ) ) ;
#16785 = CARTESIAN_POINT ( 'NONE',  ( -11.09026189855725164, 15.09941697557061957, 0.9457651797582804498 ) ) ;
#16786 = ORIENTED_EDGE ( 'NONE', *, *, #5205, .F. ) ;
#16787 = CYLINDRICAL_SURFACE ( 'NONE', #9466, 12.47473710546057646 ) ;
#16788 = DIRECTION ( 'NONE',  ( -0.5000000000000054401, 0.8660254037844354880, -0.000000000000000000 ) ) ;
#16789 = AXIS2_PLACEMENT_3D ( 'NONE', #3341, #9478, #17672 ) ;
#16790 = CARTESIAN_POINT ( 'NONE',  ( 227.9553588074475670, 39.88513931160575510, -14.00000000000005507 ) ) ;
#16791 = DIRECTION ( 'NONE',  ( 0.000000000000000000, 8.673617379884020681E-16, -1.000000000000000000 ) ) ;
#16792 = EDGE_CURVE ( 'NONE', #10058, #6217, #846, .T. ) ;
#16793 = ORIENTED_EDGE ( 'NONE', *, *, #14381, .F. ) ;
#16794 = ORIENTED_EDGE ( 'NONE', *, *, #12388, .T. ) ;
#16795 = EDGE_CURVE ( 'NONE', #3911, #12636, #5698, .T. ) ;
#16796 = CONICAL_SURFACE ( 'NONE', #6615, 13.07248899748297433, 0.6693469023067423196 ) ;
#16797 = PLANE ( 'NONE',  #9886 ) ;
#16798 = CARTESIAN_POINT ( 'NONE',  ( 220.2180084519553134, 35.41797800104779270, -14.00000000000005507 ) ) ;
#16799 = AXIS2_PLACEMENT_3D ( 'NONE', #17602, #11440, #6236 ) ;
#16800 = LINE ( 'NONE', #8410, #6647 ) ;
#16801 = DIRECTION ( 'NONE',  ( 1.000000000000000000, 0.000000000000000000, 0.000000000000000000 ) ) ;
#16802 = CARTESIAN_POINT ( 'NONE',  ( -35.00000000000000000, 65.00000000000000000, -12.50000000000000000 ) ) ;
#16803 = CARTESIAN_POINT ( 'NONE',  ( 198.7417246237710913, -1.385720969246587497, -16.73990883341915037 ) ) ;
#16804 = EDGE_CURVE ( 'NONE', #3452, #18781, #15172, .T. ) ;
#16805 = ORIENTED_EDGE ( 'NONE', *, *, #17348, .F. ) ;
#16806 = CARTESIAN_POINT ( 'NONE',  ( 81.73373490635979977, 63.06197297317982020, -25.35741583561241086 ) ) ;
#16807 = AXIS2_PLACEMENT_3D ( 'NONE', #5749, #15549, #9144 ) ;
#16808 = PLANE ( 'NONE',  #20165 ) ;
#16809 = VERTEX_POINT ( 'NONE', #7396 ) ;
#16810 = AXIS2_PLACEMENT_3D ( 'NONE', #16110, #19466, #19378 ) ;
#16811 = DIRECTION ( 'NONE',  ( 1.000000000000000000, -0.000000000000000000, -0.000000000000000000 ) ) ;
#16812 = CARTESIAN_POINT ( 'NONE',  ( 50.60228022274853288, 140.3106491262845736, 41.00000000000001421 ) ) ;
#16813 = CARTESIAN_POINT ( 'NONE',  ( 219.2795586678252562, 11.24462313530347757, -14.01558723443205068 ) ) ;
#16814 = EDGE_CURVE ( 'NONE', #11795, #7840, #15837, .T. ) ;
#16815 = DIRECTION ( 'NONE',  ( -0.5000000000000049960, 0.8660254037844357100, -0.000000000000000000 ) ) ;
#16816 = CARTESIAN_POINT ( 'NONE',  ( 194.7177224586705222, 20.69538101841223821, -14.00000000000005329 ) ) ;
#16817 = DIRECTION ( 'NONE',  ( 0.5000000000000037748, -0.8660254037844364872, 0.000000000000000000 ) ) ;
#16819 = ORIENTED_EDGE ( 'NONE', *, *, #2933, .F. ) ;
#16818 = EDGE_LOOP ( 'NONE', ( #7786, #19143, #9107, #18304 ) ) ;
#16820 = ORIENTED_EDGE ( 'NONE', *, *, #16264, .T. ) ;
#16821 = VERTEX_POINT ( 'NONE', #2336 ) ;
#16822 = CARTESIAN_POINT ( 'NONE',  ( 218.5817344997174416, 36.12073286365733793, -9.992950739179615738 ) ) ;
#16823 = CARTESIAN_POINT ( 'NONE',  ( 214.0136128684463301, 18.97851320364322447, -8.145074743996646660 ) ) ;
#16824 = VERTEX_POINT ( 'NONE', #13889 ) ;
#16825 = ORIENTED_EDGE ( 'NONE', *, *, #12868, .T. ) ;
#16826 = CARTESIAN_POINT ( 'NONE',  ( 195.2234364649848999, 3.828991977397862900, -12.59311507501989702 ) ) ;
#16827 = LINE ( 'NONE', #10231, #9165 ) ;
#16828 = LINE ( 'NONE', #18309, #9996 ) ;
#16829 = EDGE_LOOP ( 'NONE', ( #2874, #12474, #15492, #366 ) ) ;
#16830 = CARTESIAN_POINT ( 'NONE',  ( 85.37797649651368204, 230.0773763115391262, -0.9999999999999826805 ) ) ;
#16831 = CARTESIAN_POINT ( 'NONE',  ( 49.99529059433375267, 237.3619860023654553, 26.00000000000001776 ) ) ;
#16832 = CIRCLE ( 'NONE', #7676, 4.999999999999993783 ) ;
#16833 = FACE_OUTER_BOUND ( 'NONE', #13737, .T. ) ;
#16834 = CARTESIAN_POINT ( 'NONE',  ( 199.3181527907504744, -1.052920011872564343, -6.724618537539361895 ) ) ;
#16835 = CARTESIAN_POINT ( 'NONE',  ( -25.80684929261252236, 50.42143158553669480, -7.768010691411298296 ) ) ;
#16836 = FACE_OUTER_BOUND ( 'NONE', #4643, .T. ) ;
#16837 = ORIENTED_EDGE ( 'NONE', *, *, #11677, .T. ) ;
#16838 = CARTESIAN_POINT ( 'NONE',  ( 229.2073078381423556, 37.71669998195577733, -16.61383192937501718 ) ) ;
#16839 = PLANE ( 'NONE',  #12064 ) ;
#16840 = AXIS2_PLACEMENT_3D ( 'NONE', #20132, #10365, #7509 ) ;
#16842 = EDGE_LOOP ( 'NONE', ( #6149, #10113 ) ) ;
#16841 = ORIENTED_EDGE ( 'NONE', *, *, #10632, .F. ) ;
#16843 = CARTESIAN_POINT ( 'NONE',  ( 54.92373153686620668, 77.71199488874673023, -15.23237620472049336 ) ) ;
#16844 = VECTOR ( 'NONE', #7403, 1000.000000000000114 ) ;
#16845 = VERTEX_POINT ( 'NONE', #18764 ) ;
#16846 = VERTEX_POINT ( 'NONE', #4239 ) ;
#16847 = ORIENTED_EDGE ( 'NONE', *, *, #2260, .T. ) ;
#16848 = DIRECTION ( 'NONE',  ( -0.8660254037844363761, -0.5000000000000037748, 0.000000000000000000 ) ) ;
#16849 = CARTESIAN_POINT ( 'NONE',  ( 217.5096804110553137, 10.22278344732445809, -20.84195174293596153 ) ) ;
#16850 = ORIENTED_EDGE ( 'NONE', *, *, #1093, .F. ) ;
#16851 = ORIENTED_EDGE ( 'NONE', *, *, #8104, .T. ) ;
#16852 = CARTESIAN_POINT ( 'NONE',  ( 8.399999999999998579, 0.000000000000000000, 0.000000000000000000 ) ) ;
#16853 = B_SPLINE_CURVE_WITH_KNOTS ( 'NONE', 3,
 ( #19488, #16331, #8249, #10580 ),
 .UNSPECIFIED., .F., .F.,
 ( 4, 4 ),
 ( 5.589689327475942692E-05, 0.0009098826312574273935 ),
 .UNSPECIFIED. ) ;
#16854 = CARTESIAN_POINT ( 'NONE',  ( 157.3972143829815309, 45.33639716978955647, -6.000000000000052403 ) ) ;
#16855 = DIRECTION ( 'NONE',  ( 0.000000000000000000, 0.000000000000000000, -1.000000000000000000 ) ) ;
#16856 = VECTOR ( 'NONE', #8073, 1000.000000000000114 ) ;
#16857 = EDGE_CURVE ( 'NONE', #7001, #862, #10685, .T. ) ;
#16858 = LINE ( 'NONE', #3812, #311 ) ;
#16859 = AXIS2_PLACEMENT_3D ( 'NONE', #15833, #15940, #6165 ) ;
#16860 = DIRECTION ( 'NONE',  ( 0.000000000000000000, 0.000000000000000000, -1.000000000000000000 ) ) ;
#16861 = PLANE ( 'NONE',  #4921 ) ;
#16862 = CARTESIAN_POINT ( 'NONE',  ( 218.3428005204684723, 38.66593341313920007, -12.92165662794185010 ) ) ;
#16863 = ORIENTED_EDGE ( 'NONE', *, *, #12522, .T. ) ;
#16864 = CARTESIAN_POINT ( 'NONE',  ( -28.78409816537090293, 75.81673797948198512, -2.071606702223387941 ) ) ;
#16865 = CARTESIAN_POINT ( 'NONE',  ( 220.1387799105405918, 33.42385110241973223, -17.14987233279969203 ) ) ;
#16866 = DIRECTION ( 'NONE',  ( 0.8660254037844363761, 0.5000000000000041078, 0.000000000000000000 ) ) ;
#16867 = ORIENTED_EDGE ( 'NONE', *, *, #18247, .T. ) ;
#16868 = EDGE_CURVE ( 'NONE', #2271, #16360, #20513, .T. ) ;
#16869 = AXIS2_PLACEMENT_3D ( 'NONE', #18488, #2697, #3959 ) ;
#16870 = ORIENTED_EDGE ( 'NONE', *, *, #2416, .F. ) ;
#16871 = CONICAL_SURFACE ( 'NONE', #2319, 9.999999999999998224, 0.7853981633974561616 ) ;
#16872 = DIRECTION ( 'NONE',  ( -1.632680918566406547E-16, 1.632680918566406547E-16, -1.000000000000000000 ) ) ;
#16873 = CARTESIAN_POINT ( 'NONE',  ( -15.99999999999999289, 65.74999999999998579, 0.000000000000000000 ) ) ;
#16874 =( GEOMETRIC_REPRESENTATION_CONTEXT ( 3 ) GLOBAL_UNCERTAINTY_ASSIGNED_CONTEXT ( ( #12977 ) ) GLOBAL_UNIT_ASSIGNED_CONTEXT ( ( #9407, #6226, #14533 ) ) REPRESENTATION_CONTEXT ( 'NONE', 'WORKASPACE' ) );
#16875 = CARTESIAN_POINT ( 'NONE',  ( 161.8100550057988016, 307.6495024562876210, -149.9952441832748491 ) ) ;
#16876 = EDGE_CURVE ( 'NONE', #4281, #7667, #10794, .T. ) ;
#16877 = CARTESIAN_POINT ( 'NONE',  ( 229.6562112517626417, 36.61270738590849305, -13.53336351278500160 ) ) ;
#16878 = ORIENTED_EDGE ( 'NONE', *, *, #2234, .F. ) ;
#16879 = CARTESIAN_POINT ( 'NONE',  ( 75.21428198808020227, 52.24336229720762503, -15.09414418353362031 ) ) ;
#16880 = ADVANCED_FACE ( 'NONE', ( #12825 ), #7337, .T. ) ;
#16881 = CARTESIAN_POINT ( 'NONE',  ( -16.52214123053562744, 80.00000332749893062, -12.49385289755934991 ) ) ;
#16882 = DIRECTION ( 'NONE',  ( -1.000000000000000000, 0.000000000000000000, -0.000000000000000000 ) ) ;
#16883 = CARTESIAN_POINT ( 'NONE',  ( 214.0593366061550569, 19.00491181591769418, -13.97827067520052324 ) ) ;
#16884 = AXIS2_PLACEMENT_3D ( 'NONE', #14156, #20701, #1205 ) ;
#16885 = CARTESIAN_POINT ( 'NONE',  ( 220.2724395048348072, 33.19234589418308445, -10.22226263383621969 ) ) ;
#16886 = PRODUCT_DEFINITION_FORMATION_WITH_SPECIFIED_SOURCE ( 'ANY', '', #10591, .NOT_KNOWN. ) ;
#16887 = CARTESIAN_POINT ( 'NONE',  ( 208.0983737146324870, 5.661548828456886895, -14.00000000000005507 ) ) ;
#16888 = LINE ( 'NONE', #15635, #15189 ) ;
#16889 = VERTEX_POINT ( 'NONE', #16113 ) ;
#16890 = DIRECTION ( 'NONE',  ( 0.8660254037844373753, 0.5000000000000021094, -5.551115123125781716E-16 ) ) ;
#16891 = PRODUCT_DEFINITION ( 'UNKNOWN', '', #15882, #1319 ) ;
#16892 = CARTESIAN_POINT ( 'NONE',  ( 196.1782232529825762, 4.026199028858075124, -19.61257667712936126 ) ) ;
#16893 = LINE ( 'NONE', #5954, #19577 ) ;
#16894 = EDGE_CURVE ( 'NONE', #17359, #19103, #7923, .T. ) ;
#16896 = ORIENTED_EDGE ( 'NONE', *, *, #1582, .F. ) ;
#16895 = ORIENTED_EDGE ( 'NONE', *, *, #10661, .F. ) ;
#16897 = ORIENTED_EDGE ( 'NONE', *, *, #6384, .T. ) ;
#16898 = CARTESIAN_POINT ( 'NONE',  ( 204.4254563108872844, 13.44278843410413771, -0.8632678296711639998 ) ) ;
#16899 = CARTESIAN_POINT ( 'NONE',  ( 202.6391622872795324, 8.287473181319668925, -2.669358488461094581 ) ) ;
#16900 = FACE_OUTER_BOUND ( 'NONE', #11281, .T. ) ;
#16901 = EDGE_CURVE ( 'NONE', #18151, #15334, #18969, .T. ) ;
#16902 = CARTESIAN_POINT ( 'NONE',  ( 79.60733510696749704, 50.17557044886655149, -16.34883357536578785 ) ) ;
#16903 = DIRECTION ( 'NONE',  ( -0.000000000000000000, 1.000000000000000000, -0.000000000000000000 ) ) ;
#16904 = ADVANCED_FACE ( 'NONE', ( #2862 ), #11016, .T. ) ;
#16905 = ORIENTED_EDGE ( 'NONE', *, *, #11206, .F. ) ;
#16906 = CARTESIAN_POINT ( 'NONE',  ( 81.70322370085452235, 65.10829061386586147, -25.50491105577044237 ) ) ;
#16907 = CARTESIAN_POINT ( 'NONE',  ( 217.4610193877672941, 9.421868901786666584, -7.448751785191543462 ) ) ;
#16908 = B_SPLINE_CURVE_WITH_KNOTS ( 'NONE', 3,
 ( #1471, #14528, #8017, #12821 ),
 .UNSPECIFIED., .F., .F.,
 ( 4, 4 ),
 ( 0.0003733324143565315990, 0.0006786237464731411642 ),
 .UNSPECIFIED. ) ;
#16909 = ADVANCED_FACE ( 'NONE', ( #11118 ), #17272, .T. ) ;
#16910 = AXIS2_PLACEMENT_3D ( 'NONE', #5678, #12169, #18633 ) ;
#16911 = ORIENTED_EDGE ( 'NONE', *, *, #9247, .F. ) ;
#16912 = CARTESIAN_POINT ( 'NONE',  ( 202.8024860698635337, 24.48684974555284910, -15.30893474520620501 ) ) ;
#16913 = CARTESIAN_POINT ( 'NONE',  ( 219.6825814552442750, 34.21401000532726755, -17.48830818005197330 ) ) ;
#16914 = DIRECTION ( 'NONE',  ( 0.000000000000000000, 0.000000000000000000, 1.000000000000000000 ) ) ;
#16915 = DIRECTION ( 'NONE',  ( -0.5000000000000008882, 0.8660254037844381525, 0.000000000000000000 ) ) ;
#16916 = DIRECTION ( 'NONE',  ( 0.000000000000000000, 6.938893903907177533E-18, 1.000000000000000000 ) ) ;
#16917 = ORIENTED_EDGE ( 'NONE', *, *, #9866, .F. ) ;
#16918 = ORIENTED_EDGE ( 'NONE', *, *, #11349, .F. ) ;
#16919 = FACE_OUTER_BOUND ( 'NONE', #8505, .T. ) ;
#16920 = CARTESIAN_POINT ( 'NONE',  ( 196.9688168050317643, 9.137695608148359128, -3.480441514389557955 ) ) ;
#16921 = EDGE_CURVE ( 'NONE', #18021, #17399, #1580, .T. ) ;
#16922 = ORIENTED_EDGE ( 'NONE', *, *, #1006, .T. ) ;
#16923 = ORIENTED_EDGE ( 'NONE', *, *, #6210, .F. ) ;
#16924 = VERTEX_POINT ( 'NONE', #9297 ) ;
#16925 = LINE ( 'NONE', #4098, #1115 ) ;
#16926 = DIRECTION ( 'NONE',  ( 0.000000000000000000, 0.000000000000000000, -1.000000000000000000 ) ) ;
#16927 = CARTESIAN_POINT ( 'NONE',  ( 214.9383172013976093, 8.738206206044257129, -4.003039906354144861 ) ) ;
#16928 = DIRECTION ( 'NONE',  ( -0.3505956610260388406, -0.6825246866719044680, -0.6412821021618595463 ) ) ;
#16929 = CARTESIAN_POINT ( 'NONE',  ( 208.8127379954726166, 11.49776219695108814, -25.79243801023037008 ) ) ;
#16930 = EDGE_CURVE ( 'NONE', #14524, #578, #14466, .T. ) ;
#16931 = EDGE_CURVE ( 'NONE', #16603, #11936, #12450, .T. ) ;
#16932 = AXIS2_PLACEMENT_3D ( 'NONE', #15578, #15785, #1253 ) ;
#16933 = CARTESIAN_POINT ( 'NONE',  ( 221.6641179803099249, 32.29539445528372710, -12.98880265512673304 ) ) ;
#16934 = EDGE_CURVE ( 'NONE', #8261, #7581, #12413, .T. ) ;
#16935 = EDGE_CURVE ( 'NONE', #4880, #17792, #3974, .T. ) ;
#16936 = CARTESIAN_POINT ( 'NONE',  ( 221.0877080325905979, 32.36502339222965219, -14.00000000000005507 ) ) ;
#16937 = CARTESIAN_POINT ( 'NONE',  ( -23.58898520603824167, 49.74445733756040511, -9.939908570437406610 ) ) ;
#16938 = FACE_OUTER_BOUND ( 'NONE', #19739, .T. ) ;
#16939 = CARTESIAN_POINT ( 'NONE',  ( 209.3878836909736663, 4.760841834038437526, -25.81526893633800412 ) ) ;
#16940 = EDGE_CURVE ( 'NONE', #600, #14158, #9513, .T. ) ;
#16941 = DIRECTION ( 'NONE',  ( 0.5000000000000054401, -0.8660254037844354880, 0.000000000000000000 ) ) ;
#16943 = ORIENTED_EDGE ( 'NONE', *, *, #5399, .T. ) ;
#16942 = ORIENTED_EDGE ( 'NONE', *, *, #18610, .F. ) ;
#16944 = CONICAL_SURFACE ( 'NONE', #7439, 4.509097725792825528, 0.5235987755983015912 ) ;
#16945 = CARTESIAN_POINT ( 'NONE',  ( 203.3160137783235371, 23.93889567138195673, -13.80219421229064736 ) ) ;
#16946 = CARTESIAN_POINT ( 'NONE',  ( 61.88036088246662558, 82.95721218253052598, -18.86925204637720555 ) ) ;
#16947 = EDGE_CURVE ( 'NONE', #3452, #15824, #15500, .T. ) ;
#16948 = VERTEX_POINT ( 'NONE', #3167 ) ;
#16949 = ORIENTED_EDGE ( 'NONE', *, *, #11663, .F. ) ;
#16950 = ORIENTED_EDGE ( 'NONE', *, *, #16921, .T. ) ;
#16951 = CARTESIAN_POINT ( 'NONE',  ( 0.000000000000000000, 5.000000000000000000, 0.000000000000000000 ) ) ;
#16952 = FACE_OUTER_BOUND ( 'NONE', #14927, .T. ) ;
#16953 = VECTOR ( 'NONE', #2331, 1000.000000000000000 ) ;
#16954 = B_SPLINE_CURVE_WITH_KNOTS ( 'NONE', 3,
 ( #663, #8609, #6804, #13291 ),
 .UNSPECIFIED., .F., .F.,
 ( 4, 4 ),
 ( 3.205833042646720115E-07, 0.0004523738250841316598 ),
 .UNSPECIFIED. ) ;
#16955 = ORIENTED_EDGE ( 'NONE', *, *, #4953, .T. ) ;
#16956 = ORIENTED_EDGE ( 'NONE', *, *, #4997, .F. ) ;
#16957 = DIRECTION ( 'NONE',  ( -0.1005394128318080893, -0.05804645706261214733, 0.9932383577419439113 ) ) ;
#16958 = ORIENTED_EDGE ( 'NONE', *, *, #17585, .T. ) ;
#16959 = ADVANCED_FACE ( 'NONE', ( #14002 ), #16208, .F. ) ;
#16960 = VECTOR ( 'NONE', #11781, 1000.000000000000114 ) ;
#16961 = CARTESIAN_POINT ( 'NONE',  ( 218.5491876009870680, 37.69061213431084667, -11.78314368930802303 ) ) ;
#16962 = AXIS2_PLACEMENT_3D ( 'NONE', #5940, #9026, #15526 ) ;
#16963 = FACE_OUTER_BOUND ( 'NONE', #8285, .T. ) ;
#16964 = AXIS2_PLACEMENT_3D ( 'NONE', #7754, #19114, #17312 ) ;
#16965 = AXIS2_PLACEMENT_3D ( 'NONE', #19826, #13275, #19614 ) ;
#16966 = CARTESIAN_POINT ( 'NONE',  ( -12.23590939273504041, 18.40648074834063053, 11.92219499127797810 ) ) ;
#16967 = AXIS2_PLACEMENT_3D ( 'NONE', #8111, #397, #6521 ) ;
#16968 = CARTESIAN_POINT ( 'NONE',  ( 219.0841311483638947, 10.35897291369198747, -15.40190399002830723 ) ) ;
#16969 = LINE ( 'NONE', #14010, #9986 ) ;
#16970 = DIRECTION ( 'NONE',  ( 1.000000000000000000, -0.000000000000000000, -0.000000000000000000 ) ) ;
#16971 = VERTEX_POINT ( 'NONE', #16515 ) ;
#16972 = DIRECTION ( 'NONE',  ( -1.000000000000000000, -0.000000000000000000, -0.000000000000000000 ) ) ;
#16973 = CARTESIAN_POINT ( 'NONE',  ( 202.4338800647615528, 1.003545192306245282, -4.273921076953224762 ) ) ;
#16974 = CYLINDRICAL_SURFACE ( 'NONE', #7159, 5.000000000000005329 ) ;
#16975 = ORIENTED_EDGE ( 'NONE', *, *, #19951, .F. ) ;
#16976 = DIRECTION ( 'NONE',  ( 0.8660254037844362651, 0.5000000000000038858, 0.000000000000000000 ) ) ;
#16977 = VECTOR ( 'NONE', #20079, 1000.000000000000000 ) ;
#16978 = EDGE_CURVE ( 'NONE', #2929, #19916, #4856, .T. ) ;
#16979 = ORIENTED_EDGE ( 'NONE', *, *, #4244, .F. ) ;
#16980 = CARTESIAN_POINT ( 'NONE',  ( 217.4465006036304260, 9.413486477856961798, -20.57673792763531040 ) ) ;
#16981 = DIRECTION ( 'NONE',  ( 0.5000000000000051070, -0.8660254037844359321, 0.000000000000000000 ) ) ;
#16982 = AXIS2_PLACEMENT_3D ( 'NONE', #9088, #4542, #20439 ) ;
#16983 = CIRCLE ( 'NONE', #6130, 3.619616396367202782 ) ;
#16984 = CARTESIAN_POINT ( 'NONE',  ( 0.000000000000000000, 0.000000000000000000, 0.000000000000000000 ) ) ;
#16985 = CARTESIAN_POINT ( 'NONE',  ( 191.5478494775925640, 36.18576207517880050, -14.00000000000006395 ) ) ;
#16986 = ORIENTED_EDGE ( 'NONE', *, *, #9487, .F. ) ;
#16987 = CARTESIAN_POINT ( 'NONE',  ( 75.03586402968051061, 52.00729864744448605, -13.05716366695459918 ) ) ;
#16988 = LINE ( 'NONE', #2469, #8407 ) ;
#16989 = DIRECTION ( 'NONE',  ( -0.000000000000000000, -0.000000000000000000, 1.000000000000000000 ) ) ;
#16990 = CARTESIAN_POINT ( 'NONE',  ( 10.40000000000000036, 6.123233995736767268E-16, -5.000000000000000888 ) ) ;
#16991 = ORIENTED_EDGE ( 'NONE', *, *, #18766, .F. ) ;
#16992 = B_SPLINE_CURVE_WITH_KNOTS ( 'NONE', 3,
 ( #8587, #8798, #18662, #10156 ),
 .UNSPECIFIED., .F., .F.,
 ( 4, 4 ),
 ( 2.677606294903084420E-05, 0.0005927022852413137144 ),
 .UNSPECIFIED. ) ;
#16993 = CARTESIAN_POINT ( 'NONE',  ( 199.2144802262915846, 21.04890371929339921, -14.00000000000005507 ) ) ;
#16994 = CONICAL_SURFACE ( 'NONE', #3107, 10.85470691220533190, 0.8171114040043576665 ) ;
#16995 = AXIS2_PLACEMENT_3D ( 'NONE', #16259, #4704, #11175 ) ;
#16996 = VECTOR ( 'NONE', #14428, 1000.000000000000114 ) ;
#16997 = CARTESIAN_POINT ( 'NONE',  ( 208.0983737146324870, 5.661548828456886895, -14.00000000000005507 ) ) ;
#16998 = LINE ( 'NONE', #17103, #10068 ) ;
#16999 = ORIENTED_EDGE ( 'NONE', *, *, #2100, .F. ) ;
#17000 = B_SPLINE_CURVE_WITH_KNOTS ( 'NONE', 3,
 ( #20182, #794, #2275, #6923 ),
 .UNSPECIFIED., .F., .F.,
 ( 4, 4 ),
 ( 1.153766210520279721E-05, 0.0005774638844030657121 ),
 .UNSPECIFIED. ) ;
#17001 = CARTESIAN_POINT ( 'NONE',  ( 226.3265197530485864, 42.70637131117754848, -15.46846178913018122 ) ) ;
#17002 = CARTESIAN_POINT ( 'NONE',  ( -35.00000000000000000, 65.74999999999997158, 75.00000000000000000 ) ) ;
#17003 = EDGE_CURVE ( 'NONE', #14589, #3522, #552, .T. ) ;
#17004 = DIRECTION ( 'NONE',  ( 0.8660254037844370423, 0.5000000000000026645, -0.000000000000000000 ) ) ;
#17005 = CARTESIAN_POINT ( 'NONE',  ( 172.3972143829817014, 19.35563505625649583, -14.00000000000007461 ) ) ;
#17007 = ORIENTED_EDGE ( 'NONE', *, *, #20692, .T. ) ;
#17006 = VERTEX_POINT ( 'NONE', #193 ) ;
#17008 = VERTEX_POINT ( 'NONE', #9820 ) ;
#17009 = CARTESIAN_POINT ( 'NONE',  ( -11.03318111385504707, 14.43719822709678802, 11.47107871140386415 ) ) ;
#17010 = DIRECTION ( 'NONE',  ( -1.000000000000000000, -0.000000000000000000, -0.000000000000000000 ) ) ;
#17011 = VERTEX_POINT ( 'NONE', #6637 ) ;
#17012 = AXIS2_PLACEMENT_3D ( 'NONE', #19111, #2997, #11672 ) ;
#17013 = AXIS2_PLACEMENT_3D ( 'NONE', #15374, #7179, #3677 ) ;
#17014 = DIRECTION ( 'NONE',  ( -0.9885408208161388099, 0.000000000000000000, -0.1509537862398780406 ) ) ;
#17015 = CARTESIAN_POINT ( 'NONE',  ( -29.99999999999999645, 4.999999999999999112, -1.892809692664370491 ) ) ;
#17016 = PLANE ( 'NONE',  #12358 ) ;
#17017 = EDGE_LOOP ( 'NONE', ( #5229, #19764, #11765, #8353 ) ) ;
#17018 = ORIENTED_EDGE ( 'NONE', *, *, #19914, .F. ) ;
#17019 = EDGE_CURVE ( 'NONE', #11314, #1051, #8232, .T. ) ;
#17020 = CARTESIAN_POINT ( 'NONE',  ( 81.01504177493372083, 54.16268467661828367, -21.86446114789482920 ) ) ;
#17021 = DIRECTION ( 'NONE',  ( -0.9170191824714367668, 0.000000000000000000, 0.3988431007042967935 ) ) ;
#17022 = ORIENTED_EDGE ( 'NONE', *, *, #20882, .T. ) ;
#17023 = CARTESIAN_POINT ( 'NONE',  ( 209.1514512894396489, 12.04734498975750512, -15.55037597655807069 ) ) ;
#17024 = CARTESIAN_POINT ( 'NONE',  ( -0.1835734997365038312, 64.12228024131808013, 2.492032687065257601 ) ) ;
#17025 = AXIS2_PLACEMENT_3D ( 'NONE', #7519, #18876, #9208 ) ;
#17026 = CARTESIAN_POINT ( 'NONE',  ( 97.00490953756779788, 125.9389375482329569, 55.99999999999997868 ) ) ;
#17027 = EDGE_CURVE ( 'NONE', #14385, #5668, #19532, .T. ) ;
#17028 = CARTESIAN_POINT ( 'NONE',  ( 215.1183575532813848, 35.36044452787341896, -14.00000000000004441 ) ) ;
#17029 = CIRCLE ( 'NONE', #14674, 1.499999999999999556 ) ;
#17030 = CARTESIAN_POINT ( 'NONE',  ( 220.6654489287540741, 32.51163360410156145, -16.29291827778590829 ) ) ;
#17031 = EDGE_CURVE ( 'NONE', #6893, #15512, #6661, .T. ) ;
#17032 = ORIENTED_EDGE ( 'NONE', *, *, #3144, .T. ) ;
#17033 = VERTEX_POINT ( 'NONE', #13132 ) ;
#17034 = DIRECTION ( 'NONE',  ( 0.2883401610574337637, -0.4994198088140723857, -0.8169698930104393186 ) ) ;
#17035 = CARTESIAN_POINT ( 'NONE',  ( -28.48915680482256008, 80.00000000000000000, 0.5205403966592370146 ) ) ;
#17036 = ORIENTED_EDGE ( 'NONE', *, *, #14220, .F. ) ;
#17037 = EDGE_LOOP ( 'NONE', ( #3191, #3875, #13536 ) ) ;
#17038 = ORIENTED_EDGE ( 'NONE', *, *, #3165, .T. ) ;
#17039 =( NAMED_UNIT ( * ) PLANE_ANGLE_UNIT ( ) SI_UNIT ( $, .RADIAN. ) );
#17040 = PRODUCT_DEFINITION_SHAPE ( 'NONE', 'NONE',  #12880 ) ;
#17041 = CARTESIAN_POINT ( 'NONE',  ( -31.74999999999995737, 0.000000000000000000, 0.000000000000000000 ) ) ;
#17042 = CARTESIAN_POINT ( 'NONE',  ( 197.4175317442008577, -2.150244084725486005, -14.05525385477288047 ) ) ;
#17043 = EDGE_CURVE ( 'NONE', #14727, #7529, #6533, .T. ) ;
#17044 = CARTESIAN_POINT ( 'NONE',  ( 183.9132435853528307, 37.55142300003367950, -14.00000000000003730 ) ) ;
#17045 = CARTESIAN_POINT ( 'NONE',  ( -19.21593171750998863, 70.00183809964329384, -3.834978693179198928 ) ) ;
#17046 = AXIS2_PLACEMENT_3D ( 'NONE', #4531, #17679, #1663 ) ;
#17047 = DIRECTION ( 'NONE',  ( 0.7071067811865420216, 0.000000000000000000, -0.7071067811865531239 ) ) ;
#17048 = ADVANCED_FACE ( 'NONE', ( #100 ), #19865, .F. ) ;
#17049 = CARTESIAN_POINT ( 'NONE',  ( 208.8107687779841228, 4.427644383670616079, -14.00000000000005507 ) ) ;
#17050 = CARTESIAN_POINT ( 'NONE',  ( -13.26898700413883958, 45.53651568644503556, -12.21732978123357505 ) ) ;
#17051 = DIRECTION ( 'NONE',  ( -1.000000000000000000, -0.000000000000000000, -0.000000000000000000 ) ) ;
#17052 = ADVANCED_FACE ( 'NONE', ( #18108 ), #19575, .T. ) ;
#17053 = DIRECTION ( 'NONE',  ( -0.5000000000000054401, 0.8660254037844354880, -0.000000000000000000 ) ) ;
#17054 = CARTESIAN_POINT ( 'NONE',  ( -27.33357274664675884, 62.70188032564514913, 5.273416595308242805 ) ) ;
#17056 = VERTEX_POINT ( 'NONE', #18008 ) ;
#17055 = ORIENTED_EDGE ( 'NONE', *, *, #5054, .T. ) ;
#17057 = ORIENTED_EDGE ( 'NONE', *, *, #13668, .T. ) ;
#17058 = VECTOR ( 'NONE', #19102, 1000.000000000000114 ) ;
#17059 = DIRECTION ( 'NONE',  ( -0.6946590618905487124, -0.4010615963775265858, -0.5971585917027844026 ) ) ;
#17060 = APPLICATION_CONTEXT ( 'automotive_design' ) ;
#17061 = VECTOR ( 'NONE', #3455, 1000.000000000000114 ) ;
#17062 = CARTESIAN_POINT ( 'NONE',  ( 56.36150222382281783, 77.10042895211010716, -17.25692959166989837 ) ) ;
#17063 = ORIENTED_EDGE ( 'NONE', *, *, #16288, .T. ) ;
#17064 = ORIENTED_EDGE ( 'NONE', *, *, #9017, .F. ) ;
#17065 = CARTESIAN_POINT ( 'NONE',  ( 227.2691084564512778, 40.42080065374079823, -17.72162118442980372 ) ) ;
#17066 = CARTESIAN_POINT ( 'NONE',  ( 1.494606444039509041, 52.93669486463471685, -3.576234255370625448 ) ) ;
#17067 = CARTESIAN_POINT ( 'NONE',  ( -46.99999999999998579, 65.74999999999995737, -2.528164662410434804 ) ) ;
#17068 = ADVANCED_FACE ( 'NONE', ( #1994 ), #8341, .F. ) ;
#17069 = ADVANCED_FACE ( 'NONE', ( #3477 ), #14945, .F. ) ;
#17070 = ORIENTED_EDGE ( 'NONE', *, *, #14975, .F. ) ;
#17071 = ORIENTED_EDGE ( 'NONE', *, *, #16231, .T. ) ;
#17072 = DIRECTION ( 'NONE',  ( 0.8660254037844362651, 0.5000000000000042188, -6.872020471724000490E-17 ) ) ;
#17073 = VERTEX_POINT ( 'NONE', #10124 ) ;
#17074 = LINE ( 'NONE', #20233, #1623 ) ;
#17075 = DIRECTION ( 'NONE',  ( -0.4999999999999995004, 0.8660254037844390407, 0.000000000000000000 ) ) ;
#17076 = DIRECTION ( 'NONE',  ( 0.8660254037844370423, 0.5000000000000026645, -0.000000000000000000 ) ) ;
#17077 = ADVANCED_FACE ( 'NONE', ( #19469 ), #16619, .F. ) ;
#17078 = CARTESIAN_POINT ( 'NONE',  ( 218.3356494533592240, 38.67831942470078843, -15.02729838650890315 ) ) ;
#17079 = CARTESIAN_POINT ( 'NONE',  ( 220.0980799571771058, 35.62570024727892104, -17.89498551959672312 ) ) ;
#17080 = CARTESIAN_POINT ( 'NONE',  ( 0.000000000000000000, 4.685197434473814759, -6.938893903907228378E-15 ) ) ;
#17081 = CARTESIAN_POINT ( 'NONE',  ( -28.92569456491105484, 72.33610889978091052, 0.5975377147109768305 ) ) ;
#17082 = FACE_OUTER_BOUND ( 'NONE', #2091, .T. ) ;
#17083 = PLANE ( 'NONE',  #5469 ) ;
#17084 = ORIENTED_EDGE ( 'NONE', *, *, #1093, .T. ) ;
#17085 = EDGE_CURVE ( 'NONE', #19103, #4227, #14532, .T. ) ;
#17086 = VECTOR ( 'NONE', #18429, 1000.000000000000000 ) ;
#17087 = CARTESIAN_POINT ( 'NONE',  ( 81.40012587587739290, 55.32114690216545938, -2.271216619685866522 ) ) ;
#17088 = VERTEX_POINT ( 'NONE', #4957 ) ;
#17089 = ORIENTED_EDGE ( 'NONE', *, *, #19516, .T. ) ;
#17090 = CARTESIAN_POINT ( 'NONE',  ( 205.8264633344831225, 9.596613037118636669, -14.00000000000005507 ) ) ;
#17091 = CIRCLE ( 'NONE', #4218, 3.309499999999999886 ) ;
#17092 = DIRECTION ( 'NONE',  ( 0.000000000000000000, 1.000000000000000000, -1.110768649713242108E-15 ) ) ;
#17093 = DIRECTION ( 'NONE',  ( 1.000000000000000000, 0.000000000000000000, 0.000000000000000000 ) ) ;
#17094 = CARTESIAN_POINT ( 'NONE',  ( -29.99999999999999645, 9.999999999999994671, -10.49999999999999822 ) ) ;
#17095 = VERTEX_POINT ( 'NONE', #1789 ) ;
#17096 = DIRECTION ( 'NONE',  ( -0.3654179821390644567, 0.6329225110641519825, 0.6825531432186526803 ) ) ;
#17097 = LINE ( 'NONE', #18577, #8057 ) ;
#17098 = CARTESIAN_POINT ( 'NONE',  ( -15.99999999999999289, 15.09941697557068530, 15.00000000000000000 ) ) ;
#17099 = CARTESIAN_POINT ( 'NONE',  ( 229.7041009120731587, 36.85622913705960002, -14.93232347545832539 ) ) ;
#17100 = CARTESIAN_POINT ( 'NONE',  ( 51.15554463217806358, 255.3523670591321206, -8.999999999999934275 ) ) ;
#17101 = CARTESIAN_POINT ( 'NONE',  ( 215.6932043811731603, 15.82422789824195242, -11.22353489230414958 ) ) ;
#17102 = CIRCLE ( 'NONE', #5915, 12.47473710546057823 ) ;
#17103 = CARTESIAN_POINT ( 'NONE',  ( 219.1487326806684734, 35.13866320645098540, -10.43865930680574827 ) ) ;
#17104 = ORIENTED_EDGE ( 'NONE', *, *, #18844, .F. ) ;
#17105 = DIRECTION ( 'NONE',  ( -0.8660254037844378194, -0.5000000000000013323, -0.000000000000000000 ) ) ;
#17106 = DIRECTION ( 'NONE',  ( 0.8571673007021120005, 0.000000000000000000, 0.5150380749100547106 ) ) ;
#17107 = DIRECTION ( 'NONE',  ( 0.5000000000000057732, -0.8660254037844352659, -4.857225732735059248E-17 ) ) ;
#17108 = DIRECTION ( 'NONE',  ( 0.1992005449231190328, -0.3450254647022464871, 0.9172113015054553786 ) ) ;
#17110 = VERTEX_POINT ( 'NONE', #13236 ) ;
#17109 = ORIENTED_EDGE ( 'NONE', *, *, #17591, .T. ) ;
#17111 = EDGE_LOOP ( 'NONE', ( #10251, #1669, #2639, #16589 ) ) ;
#17112 = CARTESIAN_POINT ( 'NONE',  ( -11.00000000000000355, 14.76511876738014628, 11.45643923738960623 ) ) ;
#17113 = ORIENTED_EDGE ( 'NONE', *, *, #11750, .T. ) ;
#17114 = VECTOR ( 'NONE', #408, 1000.000000000000000 ) ;
#17115 = DIRECTION ( 'NONE',  ( 0.1503837331804321054, 0.08682408883346430517, -0.9848077530122086864 ) ) ;
#17116 = AXIS2_PLACEMENT_3D ( 'NONE', #4045, #12334, #2361 ) ;
#17117 = DIRECTION ( 'NONE',  ( 0.6299240516454603922, 0.3636868207865314173, 0.6862416378687268281 ) ) ;
#17118 = VECTOR ( 'NONE', #18034, 1000.000000000000000 ) ;
#17119 = CARTESIAN_POINT ( 'NONE',  ( 220.2180084519553134, 35.41797800104779270, -14.00000000000005507 ) ) ;
#17120 = EDGE_CURVE ( 'NONE', #16283, #1462, #10133, .T. ) ;
#17121 = FACE_OUTER_BOUND ( 'NONE', #6260, .T. ) ;
#17122 = ORIENTED_EDGE ( 'NONE', *, *, #467, .T. ) ;
#17123 = CARTESIAN_POINT ( 'NONE',  ( 195.9574494032261498, 8.553782366466350595, -23.53124788243903964 ) ) ;
#17124 = CYLINDRICAL_SURFACE ( 'NONE', #9717, 7.155882939242646401 ) ;
#17125 = VECTOR ( 'NONE', #15871, 1000.000000000000114 ) ;
#17126 = CARTESIAN_POINT ( 'NONE',  ( 34.99529059433364608, 263.3427481158985302, -28.99999999999997513 ) ) ;
#17127 = CARTESIAN_POINT ( 'NONE',  ( 227.9411836731248115, 38.93022547339379003, -17.81526153211079588 ) ) ;
#17128 = LINE ( 'NONE', #13850, #13051 ) ;
#17129 = CIRCLE ( 'NONE', #4268, 11.98469917212512215 ) ;
#17131 = EDGE_LOOP ( 'NONE', ( #12298, #214, #4642, #14192 ) ) ;
#17130 = ORIENTED_EDGE ( 'NONE', *, *, #20148, .T. ) ;
#17132 = EDGE_LOOP ( 'NONE', ( #8110, #16463, #12556, #11515, #11224, #6974, #20743 ) ) ;
#17133 = VECTOR ( 'NONE', #13456, 1000.000000000000114 ) ;
#17134 = CARTESIAN_POINT ( 'NONE',  ( 9.014528480800532151, 248.3427481158983596, -28.99999999999997513 ) ) ;
#17135 = EDGE_CURVE ( 'NONE', #16137, #12179, #1279, .T. ) ;
#17136 = VERTEX_POINT ( 'NONE', #7270 ) ;
#17137 = EDGE_LOOP ( 'NONE', ( #579, #9020, #16794, #1942 ) ) ;
#17138 = CARTESIAN_POINT ( 'NONE',  ( -19.76842508384192598, 11.79734777244101984, 11.92081118759508129 ) ) ;
#17139 = CARTESIAN_POINT ( 'NONE',  ( 227.3277337522544883, 40.97221779530342189, -10.60500809762007179 ) ) ;
#17140 = LINE ( 'NONE', #5883, #5957 ) ;
#17141 = CARTESIAN_POINT ( 'NONE',  ( 211.9556053886519749, 4.903475301695560340, -14.00000000000005507 ) ) ;
#17142 = FACE_OUTER_BOUND ( 'NONE', #11375, .T. ) ;
#17143 = AXIS2_PLACEMENT_3D ( 'NONE', #8070, #19524, #17643 ) ;
#17144 = EDGE_CURVE ( 'NONE', #10285, #5234, #13446, .T. ) ;
#17145 = ORIENTED_EDGE ( 'NONE', *, *, #4324, .F. ) ;
#17146 = VECTOR ( 'NONE', #15259, 1000.000000000000227 ) ;
#17147 = EDGE_CURVE ( 'NONE', #6174, #8299, #3326, .T. ) ;
#17148 = AXIS2_PLACEMENT_3D ( 'NONE', #18295, #176, #18092 ) ;
#17149 = CARTESIAN_POINT ( 'NONE',  ( 199.2144802262915846, 21.04890371929339921, -14.00000000000005507 ) ) ;
#17150 = CARTESIAN_POINT ( 'NONE',  ( -16.75433277476891547, 49.50806098447029058, -12.49936755495519414 ) ) ;
#17151 = DIRECTION ( 'NONE',  ( 0.000000000000000000, 0.000000000000000000, -1.000000000000000000 ) ) ;
#17152 = PLANE ( 'NONE',  #9454 ) ;
#17153 = CARTESIAN_POINT ( 'NONE',  ( -28.46671850446983854, 50.53532148300114102, 0.9425010236277686637 ) ) ;
#17154 = EDGE_CURVE ( 'NONE', #13693, #2710, #17755, .T. ) ;
#17156 = EDGE_LOOP ( 'NONE', ( #20658, #13766, #3744, #3414 ) ) ;
#17155 = ORIENTED_EDGE ( 'NONE', *, *, #12582, .T. ) ;
#17157 = CARTESIAN_POINT ( 'NONE',  ( 199.2144802262915846, 21.04890371929339921, -14.00000000000005507 ) ) ;
#17158 = DIRECTION ( 'NONE',  ( -0.05035489893516277571, -0.02907241445523329332, 0.9983081582712688418 ) ) ;
#17159 = EDGE_LOOP ( 'NONE', ( #10437, #1473, #3572, #4176 ) ) ;
#17160 = ORIENTED_EDGE ( 'NONE', *, *, #4110, .F. ) ;
#17161 = AXIS2_PLACEMENT_3D ( 'NONE', #12843, #6148, #19098 ) ;
#17162 = ORIENTED_EDGE ( 'NONE', *, *, #13104, .F. ) ;
#17163 = CARTESIAN_POINT ( 'NONE',  ( 216.7607129495440859, 9.790366881806683352, -5.993340328401894013 ) ) ;
#17164 = CARTESIAN_POINT ( 'NONE',  ( 229.6060668553226947, 37.02602910422319837, -15.48400627342739888 ) ) ;
#17165 = CARTESIAN_POINT ( 'NONE',  ( -5.474186428702649820, 50.03685501615670006, -13.63068399189310931 ) ) ;
#17166 = DIRECTION ( 'NONE',  ( -1.000000000000000000, 0.000000000000000000, 0.000000000000000000 ) ) ;
#17167 = ORIENTED_EDGE ( 'NONE', *, *, #15000, .F. ) ;
#17168 = EDGE_CURVE ( 'NONE', #19498, #13379, #8878, .T. ) ;
#17169 = ORIENTED_EDGE ( 'NONE', *, *, #10534, .T. ) ;
#17170 = CARTESIAN_POINT ( 'NONE',  ( 215.9107784512153216, 15.77283444196598694, -16.79818413631500817 ) ) ;
#17171 = ADVANCED_FACE ( 'NONE', ( #2412 ), #14836, .T. ) ;
#17172 = CARTESIAN_POINT ( 'NONE',  ( 95.83809698076872507, 24.95991617951895236, -12.50000000000000000 ) ) ;
#17173 = CARTESIAN_POINT ( 'NONE',  ( 229.7502435232953530, 36.77630779002864614, -12.46964089162990952 ) ) ;
#17174 = AXIS2_PLACEMENT_3D ( 'NONE', #10022, #13342, #1892 ) ;
#17175 = B_SPLINE_CURVE_WITH_KNOTS ( 'NONE', 3,
 ( #7816, #17582, #12609, #17163 ),
 .UNSPECIFIED., .F., .F.,
 ( 4, 4 ),
 ( 4.835194380548316019E-05, 0.0009023376817886681828 ),
 .UNSPECIFIED. ) ;
#17176 = LINE ( 'NONE', #20553, #5456 ) ;
#17177 = CARTESIAN_POINT ( 'NONE',  ( 216.6495311407713871, 8.953355943939367734, -6.376588578941993823 ) ) ;
#17178 = DIRECTION ( 'NONE',  ( 0.5000000000000044409, -0.8660254037844360431, 0.000000000000000000 ) ) ;
#17179 = EDGE_CURVE ( 'NONE', #9209, #13744, #3808, .T. ) ;
#17180 = ORIENTED_EDGE ( 'NONE', *, *, #20653, .F. ) ;
#17181 = CARTESIAN_POINT ( 'NONE',  ( 216.5107763960967020, 15.86188268823392278, -14.01039157610429520 ) ) ;
#17182 = DIRECTION ( 'NONE',  ( -0.8660254037844360431, -0.5000000000000045519, 0.000000000000000000 ) ) ;
#17183 = CARTESIAN_POINT ( 'NONE',  ( -11.10102051443364779, 14.09941697557065332, 0.9999999999999991118 ) ) ;
#17184 = EDGE_CURVE ( 'NONE', #3711, #16338, #13656, .T. ) ;
#17185 = ORIENTED_EDGE ( 'NONE', *, *, #17768, .T. ) ;
#17186 = CARTESIAN_POINT ( 'NONE',  ( 81.65190015349629959, 63.92029392008140576, 0.4576250216425485906 ) ) ;
#17187 = ORIENTED_EDGE ( 'NONE', *, *, #11192, .T. ) ;
#17188 = ORIENTED_EDGE ( 'NONE', *, *, #18168, .F. ) ;
#17189 = CARTESIAN_POINT ( 'NONE',  ( 204.7342393044282289, 2.074058994753574581, -24.85758746085085846 ) ) ;
#17190 = CARTESIAN_POINT ( 'NONE',  ( 196.8077463644258387, 4.389654366710942668, -7.132002368301173512 ) ) ;
#17191 = EDGE_CURVE ( 'NONE', #3576, #2651, #5785, .T. ) ;
#17192 = AXIS2_PLACEMENT_3D ( 'NONE', #264, #13105, #6607 ) ;
#17193 = AXIS2_PLACEMENT_3D ( 'NONE', #19339, #8079, #14387 ) ;
#17194 = FACE_OUTER_BOUND ( 'NONE', #17238, .T. ) ;
#17195 = VERTEX_POINT ( 'NONE', #20112 ) ;
#17196 = CARTESIAN_POINT ( 'NONE',  ( -35.00000000000000000, 65.00000000000000000, -12.50000000000000000 ) ) ;
#17197 = EDGE_CURVE ( 'NONE', #11090, #11291, #15162, .T. ) ;
#17198 = CARTESIAN_POINT ( 'NONE',  ( 227.3848655466122182, 39.89379673368515711, -10.10863206319041296 ) ) ;
#17199 = DIRECTION ( 'NONE',  ( 0.000000000000000000, 0.000000000000000000, -1.000000000000000000 ) ) ;
#17200 = CARTESIAN_POINT ( 'NONE',  ( 1.484819526751601559, 76.25000000000000000, -2.578432583507792142 ) ) ;
#17201 = CARTESIAN_POINT ( 'NONE',  ( 228.4406543832519674, 38.06511682656112328, -17.45257705044836172 ) ) ;
#17202 = EDGE_CURVE ( 'NONE', #5086, #8157, #15057, .T. ) ;
#17203 = CARTESIAN_POINT ( 'NONE',  ( 205.5965122587965084, 9.994899983462953941, -14.00000000000005507 ) ) ;
#17204 = AXIS2_PLACEMENT_3D ( 'NONE', #14246, #10819, #12332 ) ;
#17205 = DIRECTION ( 'NONE',  ( 1.000000000000000000, 6.608470384673549052E-16, 0.000000000000000000 ) ) ;
#17206 = PRODUCT ( 'Middle Handle-Connected Base', 'Middle Handle-Connected Base', '', ( #17298 ) ) ;
#17207 = ORIENTED_EDGE ( 'NONE', *, *, #11828, .T. ) ;
#17208 = DIRECTION ( 'NONE',  ( -1.000000000000000000, 0.000000000000000000, 0.000000000000000000 ) ) ;
#17209 = PLANE ( 'NONE',  #371 ) ;
#17210 = CARTESIAN_POINT ( 'NONE',  ( 22.00490953756710510, 255.8427481158984733, -28.99999999999997513 ) ) ;
#17211 = CARTESIAN_POINT ( 'NONE',  ( -15.99999999999999289, 79.99999999999998579, -12.50000000000000178 ) ) ;
#17213 = VERTEX_POINT ( 'NONE', #18421 ) ;
#17212 = EDGE_LOOP ( 'NONE', ( #8217, #542, #7242, #16986 ) ) ;
#17214 = B_SPLINE_CURVE_WITH_KNOTS ( 'NONE', 3,
 ( #11408, #16191, #14822, #14508 ),
 .UNSPECIFIED., .F., .F.,
 ( 4, 4 ),
 ( 1.191936099701994174E-06, 0.0005671181583943551681 ),
 .UNSPECIFIED. ) ;
#17215 = FACE_OUTER_BOUND ( 'NONE', #5194, .T. ) ;
#17216 = FILL_AREA_STYLE_COLOUR ( '', #13622 ) ;
#17217 = ORIENTED_EDGE ( 'NONE', *, *, #18350, .T. ) ;
#17218 = PRODUCT_DEFINITION_CONTEXT ( 'detailed design', #16246, 'design' ) ;
#17219 = DIRECTION ( 'NONE',  ( 0.000000000000000000, 0.000000000000000000, 1.000000000000000000 ) ) ;
#17220 = AXIS2_PLACEMENT_3D ( 'NONE', #7118, #19840, #13708 ) ;
#17221 = LINE ( 'NONE', #8186, #1859 ) ;
#17222 = ORIENTED_EDGE ( 'NONE', *, *, #17421, .F. ) ;
#17223 = AXIS2_PLACEMENT_3D ( 'NONE', #9357, #1327, #7775 ) ;
#17224 = CARTESIAN_POINT ( 'NONE',  ( 177.1791022559528983, 56.75747545832872731, 0.9999999999999431566 ) ) ;
#17225 = CARTESIAN_POINT ( 'NONE',  ( 0.000000000000000000, 0.000000000000000000, 0.000000000000000000 ) ) ;
#17226 = ORIENTED_EDGE ( 'NONE', *, *, #19702, .F. ) ;
#17227 = DIRECTION ( 'NONE',  ( -0.5000000000000047740, 0.8660254037844358210, 0.000000000000000000 ) ) ;
#17228 = DIRECTION ( 'NONE',  ( 0.000000000000000000, 0.000000000000000000, 1.000000000000000000 ) ) ;
#17229 = CARTESIAN_POINT ( 'NONE',  ( 198.7417246237710913, -1.385720969246587497, -16.73990883341915037 ) ) ;
#17230 = CARTESIAN_POINT ( 'NONE',  ( 5.000000000000000000, 0.000000000000000000, 0.000000000000000000 ) ) ;
#17231 = CARTESIAN_POINT ( 'NONE',  ( 216.1256026380747244, 15.71984656690478310, -11.16670872502649914 ) ) ;
#17232 = AXIS2_PLACEMENT_3D ( 'NONE', #20238, #17276, #2658 ) ;
#17233 = ORIENTED_EDGE ( 'NONE', *, *, #3043, .F. ) ;
#17234 = ORIENTED_EDGE ( 'NONE', *, *, #19334, .T. ) ;
#17235 = DIRECTION ( 'NONE',  ( 0.8660254037844371533, 0.5000000000000026645, 6.106226635438360972E-16 ) ) ;
#17236 = ORIENTED_EDGE ( 'NONE', *, *, #9979, .F. ) ;
#17237 = ORIENTED_EDGE ( 'NONE', *, *, #11946, .F. ) ;
#17238 = EDGE_LOOP ( 'NONE', ( #9223, #5707, #18490, #16609, #13293, #14314 ) ) ;
#17239 = EDGE_CURVE ( 'NONE', #2539, #10247, #3889, .T. ) ;
#17240 = CARTESIAN_POINT ( 'NONE',  ( -20.33466442860505197, 12.58620624673167221, 11.72593040804455278 ) ) ;
#17241 = CARTESIAN_POINT ( 'NONE',  ( 80.86682143426207858, 53.72248789457500351, -3.489252184860733408 ) ) ;
#17242 = DIRECTION ( 'NONE',  ( 0.8660254037844361541, 0.5000000000000043299, -5.976026924694053325E-17 ) ) ;
#17243 = CARTESIAN_POINT ( 'NONE',  ( 35.35427444295658717, 182.7209698509878422, 11.00000000000001243 ) ) ;
#17244 = CARTESIAN_POINT ( 'NONE',  ( 44.00000000000000000, 0.000000000000000000, 15.00000000000000000 ) ) ;
#17245 = VERTEX_POINT ( 'NONE', #7173 ) ;
#17246 = CONICAL_SURFACE ( 'NONE', #18257, 4.509097725792825528, 0.5235987755983015912 ) ;
#17247 = CARTESIAN_POINT ( 'NONE',  ( 226.3046507595724961, 42.74424951898829761, -15.48400627342726921 ) ) ;
#17248 = EDGE_CURVE ( 'NONE', #14336, #6716, #4991, .T. ) ;
#17249 = CARTESIAN_POINT ( 'NONE',  ( 220.4965759700381511, 32.80413014862196519, -11.35524774226752953 ) ) ;
#17250 = CARTESIAN_POINT ( 'NONE',  ( -19.35604988386060299, 50.41666730312486777, -16.01143037413084969 ) ) ;
#17251 = CARTESIAN_POINT ( 'NONE',  ( 80.00000000000000000, 4.172000000000002373, -2.710505431213761085E-17 ) ) ;
#17252 = VECTOR ( 'NONE', #5454, 1000.000000000000227 ) ;
#17253 = DIRECTION ( 'NONE',  ( 0.000000000000000000, -0.4999999999999985567, 0.8660254037844393737 ) ) ;
#17254 = CARTESIAN_POINT ( 'NONE',  ( -27.46410040126770724, 60.39801160101181665, 4.985054410776884382 ) ) ;
#17256 = EDGE_LOOP ( 'NONE', ( #18102, #626, #11793, #7971, #13605, #17426, #6668, #13229, #17055, #7999, #345, #16005, #18101, #19486, #353, #11383 ) ) ;
#17255 = ORIENTED_EDGE ( 'NONE', *, *, #19864, .F. ) ;
#17257 = DIRECTION ( 'NONE',  ( 0.000000000000000000, 0.000000000000000000, -1.000000000000000000 ) ) ;
#17258 = B_SPLINE_CURVE_WITH_KNOTS ( 'NONE', 3,
 ( #6299, #64, #16274, #6502 ),
 .UNSPECIFIED., .F., .F.,
 ( 4, 4 ),
 ( 2.765582935369313113E-07, 0.0004523298000734190410 ),
 .UNSPECIFIED. ) ;
#17259 = DIRECTION ( 'NONE',  ( 0.5000000000000044409, -0.8660254037844360431, 0.000000000000000000 ) ) ;
#17260 = EDGE_CURVE ( 'NONE', #19392, #9907, #4325, .T. ) ;
#17261 = CARTESIAN_POINT ( 'NONE',  ( -3.499198184780732745, 80.00000000000000000, 0.2411454413945828268 ) ) ;
#17262 = ORIENTED_EDGE ( 'NONE', *, *, #7926, .T. ) ;
#17263 = ORIENTED_EDGE ( 'NONE', *, *, #7708, .F. ) ;
#17264 = EDGE_CURVE ( 'NONE', #3323, #13300, #12955, .T. ) ;
#17265 = DIRECTION ( 'NONE',  ( 0.000000000000000000, 1.000000000000000000, 0.000000000000000000 ) ) ;
#17266 = CARTESIAN_POINT ( 'NONE',  ( 229.3155625773928250, 36.54973138235077812, -15.57898118447804769 ) ) ;
#17267 = CARTESIAN_POINT ( 'NONE',  ( -26.56874857031798598, 50.03503563072523974, -13.60624899383130071 ) ) ;
#17268 = CARTESIAN_POINT ( 'NONE',  ( 227.9553588074475954, 39.88513931160571957, -14.00000000000005507 ) ) ;
#17269 = VERTEX_POINT ( 'NONE', #17244 ) ;
#17270 = VECTOR ( 'NONE', #175, 1000.000000000000114 ) ;
#17271 = ORIENTED_EDGE ( 'NONE', *, *, #12286, .F. ) ;
#17272 = PLANE ( 'NONE',  #19201 ) ;
#17273 = EDGE_LOOP ( 'NONE', ( #10280, #19672, #16841, #17852 ) ) ;
#17274 = CARTESIAN_POINT ( 'NONE',  ( 214.8766030929655813, 15.35276292467472103, -19.36714384557541990 ) ) ;
#17275 = DIRECTION ( 'NONE',  ( 0.5000000000000049960, -0.8660254037844358210, 0.000000000000000000 ) ) ;
#17276 = DIRECTION ( 'NONE',  ( -0.5000000000000049960, 0.8660254037844357100, -0.000000000000000000 ) ) ;
#17277 = PRODUCT_RELATED_PRODUCT_CATEGORY ( 'part', '', ( #10402 ) ) ;
#17278 = DIRECTION ( 'NONE',  ( -0.8660254037844380415, -0.5000000000000014433, -0.000000000000000000 ) ) ;
#17279 = DIRECTION ( 'NONE',  ( -1.000000000000000000, -0.000000000000000000, -0.000000000000000000 ) ) ;
#17280 = DIRECTION ( 'NONE',  ( -0.8660254037844370423, -0.5000000000000026645, 0.000000000000000000 ) ) ;
#17281 = MANIFOLD_SOLID_BREP ( 'Hex', #20157 ) ;
#17282 = AXIS2_PLACEMENT_3D ( 'NONE', #9236, #4590, #11270 ) ;
#17283 = CARTESIAN_POINT ( 'NONE',  ( -31.82693145428951098, 65.99841087575286736, 2.475388239833567372 ) ) ;
#17284 = VECTOR ( 'NONE', #18484, 1000.000000000000114 ) ;
#17285 = CARTESIAN_POINT ( 'NONE',  ( 27.00000000000002487, 65.00000000000000000, -27.49999999999999645 ) ) ;
#17286 = DIRECTION ( 'NONE',  ( -0.8296432542242747621, -0.4789947561577490021, 0.2868032327110942581 ) ) ;
#17287 = ORIENTED_EDGE ( 'NONE', *, *, #13945, .F. ) ;
#17288 = CARTESIAN_POINT ( 'NONE',  ( 80.41157793103774054, 67.74023943711713969, 0.5468165597092933261 ) ) ;
#17289 = TOROIDAL_SURFACE ( 'NONE', #5763, 4.400000000000000355, 0.4000000000000000222 ) ;
#17290 = ADVANCED_FACE ( 'NONE', ( #4624 ), #2304, .T. ) ;
#17291 = VERTEX_POINT ( 'NONE', #20620 ) ;
#17292 = EDGE_CURVE ( 'NONE', #6578, #491, #5988, .T. ) ;
#17293 = ORIENTED_EDGE ( 'NONE', *, *, #20128, .F. ) ;
#17294 = CARTESIAN_POINT ( 'NONE',  ( 174.8972143829816446, 15.02550803733428353, -14.00000000000000533 ) ) ;
#17295 = CARTESIAN_POINT ( 'NONE',  ( 201.0771824364471172, 22.12433534174682492, -26.28791492288521781 ) ) ;
#17296 = AXIS2_PLACEMENT_3D ( 'NONE', #20886, #10748, #12467 ) ;
#17297 = VECTOR ( 'NONE', #5726, 1000.000000000000114 ) ;
#17298 = PRODUCT_CONTEXT ( 'NONE', #16771, 'mechanical' ) ;
#17299 = AXIS2_PLACEMENT_3D ( 'NONE', #6315, #12494, #15789 ) ;
#17300 = CARTESIAN_POINT ( 'NONE',  ( 219.6466669664155233, 35.75969730707029015, -17.51488284254726935 ) ) ;
#17301 = ADVANCED_FACE ( 'NONE', ( #17142 ), #1144, .F. ) ;
#17302 = PLANE ( 'NONE',  #14514 ) ;
#17303 = CARTESIAN_POINT ( 'NONE',  ( 57.15554463217811332, 244.9600622137188850, -13.99999999999998046 ) ) ;
#17304 = CARTESIAN_POINT ( 'NONE',  ( 10.49211908931699178, -10.00000000000000000, -5.999999999999998224 ) ) ;
#17305 = CARTESIAN_POINT ( 'NONE',  ( 199.7342393044281437, 10.73431303259792813, -24.85758746085085491 ) ) ;
#17306 = CIRCLE ( 'NONE', #10178, 5.000000000000001776 ) ;
#17307 = CARTESIAN_POINT ( 'NONE',  ( 218.6471291873297673, 37.93284263396564882, -11.63296046036683329 ) ) ;
#17308 = EDGE_CURVE ( 'NONE', #18356, #9257, #15185, .T. ) ;
#17309 = VECTOR ( 'NONE', #17286, 1000.000000000000114 ) ;
#17310 = AXIS2_PLACEMENT_3D ( 'NONE', #4677, #3194, #2995 ) ;
#17311 = CARTESIAN_POINT ( 'NONE',  ( 216.5584123369822009, 15.79270668264091881, -15.43274561385901045 ) ) ;
#17312 = DIRECTION ( 'NONE',  ( 0.000000000000000000, 0.000000000000000000, -1.000000000000000000 ) ) ;
#17313 = CYLINDRICAL_SURFACE ( 'NONE', #14853, 5.999999999999989342 ) ;
#17314 = EDGE_LOOP ( 'NONE', ( #20203, #14807, #19132, #14958 ) ) ;
#17315 = AXIS2_PLACEMENT_3D ( 'NONE', #5845, #14147, #11151 ) ;
#17316 = DIRECTION ( 'NONE',  ( 1.207457829957650937E-16, -7.169742151387006041E-17, 1.000000000000000000 ) ) ;
#17317 = EDGE_CURVE ( 'NONE', #17073, #16560, #3034, .T. ) ;
#17318 = DIRECTION ( 'NONE',  ( 0.8660254037844373753, 0.5000000000000022204, 0.000000000000000000 ) ) ;
#17319 = AXIS2_PLACEMENT_3D ( 'NONE', #13855, #20303, #18728 ) ;
#17320 = CARTESIAN_POINT ( 'NONE',  ( -28.96704929677014917, 76.49637892406967410, -2.857129581998074208 ) ) ;
#17322 = ORIENTED_EDGE ( 'NONE', *, *, #4715, .T. ) ;
#17321 = ORIENTED_EDGE ( 'NONE', *, *, #19742, .T. ) ;
#17323 = DIRECTION ( 'NONE',  ( 0.000000000000000000, -1.000000000000000000, -4.616915249250367527E-16 ) ) ;
#17324 = CARTESIAN_POINT ( 'NONE',  ( 227.5312376355471145, 39.64027283883993391, -14.00000000000005507 ) ) ;
#17325 = ORIENTED_EDGE ( 'NONE', *, *, #18192, .T. ) ;
#17326 = EDGE_CURVE ( 'NONE', #1522, #11167, #284, .T. ) ;
#17327 = AXIS2_PLACEMENT_3D ( 'NONE', #8200, #3232, #1650 ) ;
#17328 = PLANE ( 'NONE',  #5618 ) ;
#17329 = EDGE_CURVE ( 'NONE', #14630, #19987, #10743, .T. ) ;
#17330 = CARTESIAN_POINT ( 'NONE',  ( 32.36389338619004263, 157.9004617752989930, -12.50000000000000000 ) ) ;
#17331 = CIRCLE ( 'NONE', #12596, 12.47473710546057823 ) ;
#17332 = AXIS2_PLACEMENT_3D ( 'NONE', #13725, #5323, #11814 ) ;
#17333 = DIRECTION ( 'NONE',  ( 0.5000000000000054401, -0.8660254037844354880, 0.000000000000000000 ) ) ;
#17334 = ORIENTED_EDGE ( 'NONE', *, *, #10976, .F. ) ;
#17335 = AXIS2_PLACEMENT_3D ( 'NONE', #4026, #12089, #15400 ) ;
#17336 = DIRECTION ( 'NONE',  ( -0.8660254037844370423, -0.5000000000000026645, 0.000000000000000000 ) ) ;
#17337 = EDGE_CURVE ( 'NONE', #3796, #19116, #9479, .T. ) ;
#17338 = ORIENTED_EDGE ( 'NONE', *, *, #7983, .T. ) ;
#17339 = CARTESIAN_POINT ( 'NONE',  ( 30.10683012259193703, 0.000000000000000000, 0.000000000000000000 ) ) ;
#17340 = CARTESIAN_POINT ( 'NONE',  ( 221.6021718675050352, 32.60860647079822172, -12.05101037009758791 ) ) ;
#17341 = FACE_OUTER_BOUND ( 'NONE', #2299, .T. ) ;
#17342 = LINE ( 'NONE', #19039, #17622 ) ;
#17343 = MECHANICAL_DESIGN_GEOMETRIC_PRESENTATION_REPRESENTATION (  '', ( #11923 ), #1094 ) ;
#17344 = VERTEX_POINT ( 'NONE', #15985 ) ;
#17345 = EDGE_LOOP ( 'NONE', ( #10339, #16896, #6370, #17817, #13202 ) ) ;
#17346 = AXIS2_PLACEMENT_3D ( 'NONE', #2666, #7835, #9105 ) ;
#17347 = CARTESIAN_POINT ( 'NONE',  ( 8.399999999999998579, 0.000000000000000000, 0.000000000000000000 ) ) ;
#17348 = EDGE_CURVE ( 'NONE', #19292, #5200, #10876, .T. ) ;
#17349 = CIRCLE ( 'NONE', #12268, 13.99999999999999822 ) ;
#17350 = AXIS2_PLACEMENT_3D ( 'NONE', #9801, #20934, #4933 ) ;
#17351 = ORIENTED_EDGE ( 'NONE', *, *, #6392, .T. ) ;
#17352 = ORIENTED_EDGE ( 'NONE', *, *, #13049, .T. ) ;
#17353 = FACE_OUTER_BOUND ( 'NONE', #20943, .T. ) ;
#17354 = CARTESIAN_POINT ( 'NONE',  ( -46.99999999999998579, 65.74999999999995737, -2.528164662410434804 ) ) ;
#17355 = DIRECTION ( 'NONE',  ( -0.8660254037844344888, -0.5000000000000069944, 0.000000000000000000 ) ) ;
#17356 = DIRECTION ( 'NONE',  ( -0.8660254037844370423, -0.5000000000000026645, 0.000000000000000000 ) ) ;
#17357 = FACE_OUTER_BOUND ( 'NONE', #179, .T. ) ;
#17358 = ADVANCED_FACE ( 'NONE', ( #17357 ), #14191, .F. ) ;
#17359 = VERTEX_POINT ( 'NONE', #13001 ) ;
#17360 = DIRECTION ( 'NONE',  ( -0.5000000000000051070, 0.8660254037844355990, 0.000000000000000000 ) ) ;
#17361 = AXIS2_PLACEMENT_3D ( 'NONE', #1926, #8589, #328 ) ;
#17362 = VECTOR ( 'NONE', #13203, 1000.000000000000114 ) ;
#17363 = SURFACE_STYLE_USAGE ( .BOTH. , #1037 ) ;
#17364 = CARTESIAN_POINT ( 'NONE',  ( -18.39717848847821813, 45.55555640428114828, -12.27279083252108016 ) ) ;
#17365 = LINE ( 'NONE', #3149, #10957 ) ;
#17366 = CARTESIAN_POINT ( 'NONE',  ( 221.6641179803099249, 32.29539445528372710, -12.98880265512673304 ) ) ;
#17367 = CARTESIAN_POINT ( 'NONE',  ( 199.6607596192359608, -0.8551158672202783251, -8.669480444820576892 ) ) ;
#17369 = ORIENTED_EDGE ( 'NONE', *, *, #208, .F. ) ;
#17368 = VERTEX_POINT ( 'NONE', #11501 ) ;
#17370 = ORIENTED_EDGE ( 'NONE', *, *, #11895, .F. ) ;
#17371 = CYLINDRICAL_SURFACE ( 'NONE', #11542, 14.99999999999999645 ) ;
#17372 = CARTESIAN_POINT ( 'NONE',  ( 205.8264633344831225, 9.596613037118636669, -14.00000000000005507 ) ) ;
#17373 = CARTESIAN_POINT ( 'NONE',  ( 1.320351081125068049, 77.22491497699002139, -3.799191488835419683 ) ) ;
#17374 = VERTEX_POINT ( 'NONE', #17879 ) ;
#17375 = VERTEX_POINT ( 'NONE', #5026 ) ;
#17376 = CARTESIAN_POINT ( 'NONE',  ( 218.9402551536602459, 37.01326326388927157, -16.94731950718122349 ) ) ;
#17377 = LINE ( 'NONE', #2857, #14947 ) ;
#17378 = CARTESIAN_POINT ( 'NONE',  ( 1.332880925387092796, 55.04869403453741938, -1.249173068972419198 ) ) ;
#17379 = CARTESIAN_POINT ( 'NONE',  ( -28.99999999999999289, 0.000000000000000000, 15.00000000000000178 ) ) ;
#17380 = ORIENTED_EDGE ( 'NONE', *, *, #5380, .F. ) ;
#17381 = EDGE_LOOP ( 'NONE', ( #3639, #7444, #1715, #16301, #3695 ) ) ;
#17382 = CARTESIAN_POINT ( 'NONE',  ( 208.0983737146324870, 5.661548828456886895, -14.00000000000005507 ) ) ;
#17383 = DIRECTION ( 'NONE',  ( 0.5000000000000049960, -0.8660254037844358210, 0.000000000000000000 ) ) ;
#17384 = FACE_OUTER_BOUND ( 'NONE', #9940, .T. ) ;
#17385 = DIRECTION ( 'NONE',  ( -0.3412765716093312807, 0.5911083614602687941, -0.7308359642781253607 ) ) ;
#17386 = CARTESIAN_POINT ( 'NONE',  ( 81.61199360759415811, 66.29268519405596294, -25.62653348100026918 ) ) ;
#17387 = ADVANCED_FACE ( 'NONE', ( #4828 ), #19354, .F. ) ;
#17388 = CARTESIAN_POINT ( 'NONE',  ( 226.9304947408143391, 41.66025594586614034, -16.98332657222546871 ) ) ;
#17389 = DIRECTION ( 'NONE',  ( -0.2483788854152945980, -0.1434016163555415502, 0.9579895123154918979 ) ) ;
#17390 = PLANE ( 'NONE',  #8905 ) ;
#17391 = CIRCLE ( 'NONE', #9241, 5.000000000000000888 ) ;
#17392 = ORIENTED_EDGE ( 'NONE', *, *, #8782, .T. ) ;
#17393 = DIRECTION ( 'NONE',  ( 0.000000000000000000, 6.938893903907178303E-18, 1.000000000000000000 ) ) ;
#17394 = DIRECTION ( 'NONE',  ( -0.5566703992264184775, -0.3213938048432737893, -0.7660444431189769032 ) ) ;
#17395 = PLANE ( 'NONE',  #2457 ) ;
#17396 = ORIENTED_EDGE ( 'NONE', *, *, #455, .F. ) ;
#17397 = CARTESIAN_POINT ( 'NONE',  ( 77.91874456701133056, 67.35752264558084335, 0.2884206837271629520 ) ) ;
#17398 = ORIENTED_EDGE ( 'NONE', *, *, #19748, .T. ) ;
#17399 = VERTEX_POINT ( 'NONE', #17673 ) ;
#17400 = CARTESIAN_POINT ( 'NONE',  ( -4.085501928355141033, 74.13367381892273045, 3.782735275915807716 ) ) ;
#17401 = CARTESIAN_POINT ( 'NONE',  ( 211.7014381176568065, 13.51958057145868253, -4.494676796018852727 ) ) ;
#17402 = EDGE_CURVE ( 'NONE', #2749, #10441, #14814, .T. ) ;
#17403 = PRODUCT_CONTEXT ( 'NONE', #927, 'mechanical' ) ;
#17404 = VECTOR ( 'NONE', #17275, 1000.000000000000227 ) ;
#17405 = AXIS2_PLACEMENT_3D ( 'NONE', #15716, #7521, #8908 ) ;
#17406 = DIRECTION ( 'NONE',  ( 0.4406902839761535629, -0.8976592190854038034, 0.000000000000000000 ) ) ;
#17407 = ORIENTED_EDGE ( 'NONE', *, *, #14866, .T. ) ;
#17408 = DIRECTION ( 'NONE',  ( 0.1933428247760533847, 0.9811312614057389192, 0.000000000000000000 ) ) ;
#17409 = CARTESIAN_POINT ( 'NONE',  ( 211.2092941256368306, 27.71181611822996160, -15.25318819445429597 ) ) ;
#17410 = CARTESIAN_POINT ( 'NONE',  ( -11.09026189855742572, 14.76386108487820259, 0.9457651797581829722 ) ) ;
#17411 = ADVANCED_FACE ( 'NONE', ( #3445 ), #16280, .F. ) ;
#17412 = EDGE_CURVE ( 'NONE', #11656, #20827, #3545, .T. ) ;
#17413 = CARTESIAN_POINT ( 'NONE',  ( 28.00000000000001066, 65.75000000000001421, 75.00000000000000000 ) ) ;
#17414 = DIRECTION ( 'NONE',  ( -1.000000000000000000, -0.000000000000000000, -0.000000000000000000 ) ) ;
#17415 = LINE ( 'NONE', #7753, #5852 ) ;
#17416 = LINE ( 'NONE', #7544, #7479 ) ;
#17417 = DIRECTION ( 'NONE',  ( -0.000000000000000000, -1.000000000000000000, -0.000000000000000000 ) ) ;
#17418 = ORIENTED_EDGE ( 'NONE', *, *, #7441, .T. ) ;
#17419 = CARTESIAN_POINT ( 'NONE',  ( 228.5962672867603374, 38.77505326243435491, -17.68583624946730737 ) ) ;
#17420 = CARTESIAN_POINT ( 'NONE',  ( 201.9636910742785005, 0.3660905863451732745, -14.00000000000005507 ) ) ;
#17421 = EDGE_CURVE ( 'NONE', #14829, #10630, #8023, .T. ) ;
#17422 = FACE_OUTER_BOUND ( 'NONE', #16257, .T. ) ;
#17423 = CARTESIAN_POINT ( 'NONE',  ( 195.2889461848653525, 4.043823935988862139, -15.40420431385919464 ) ) ;
#17424 = CARTESIAN_POINT ( 'NONE',  ( -20.89897948556633978, 14.09941697557065332, 0.9999999999999991118 ) ) ;
#17426 = ORIENTED_EDGE ( 'NONE', *, *, #20480, .T. ) ;
#17425 = ORIENTED_EDGE ( 'NONE', *, *, #15805, .T. ) ;
#17427 = CYLINDRICAL_SURFACE ( 'NONE', #749, 3.902363844300889451 ) ;
#17428 = CARTESIAN_POINT ( 'NONE',  ( 205.1848235957376403, 9.226162161231169279, -26.45271578590682893 ) ) ;
#17429 = ORIENTED_EDGE ( 'NONE', *, *, #4872, .F. ) ;
#17430 = PRODUCT_DEFINITION_CONTEXT ( 'detailed design', #4458, 'design' ) ;
#17431 = ADVANCED_FACE ( 'NONE', ( #8203 ), #14812, .F. ) ;
#17432 = DIRECTION ( 'NONE',  ( -0.8660254037844355990, -0.5000000000000055511, 0.000000000000000000 ) ) ;
#17433 = ORIENTED_EDGE ( 'NONE', *, *, #3719, .T. ) ;
#17434 = DIRECTION ( 'NONE',  ( -0.000000000000000000, 1.000000000000000000, -0.000000000000000000 ) ) ;
#17435 = VECTOR ( 'NONE', #19968, 1000.000000000000000 ) ;
#17436 = CARTESIAN_POINT ( 'NONE',  ( 195.6791760372415183, 3.738073984511642855, -9.718744748712971671 ) ) ;
#17437 = EDGE_CURVE ( 'NONE', #166, #1421, #11773, .T. ) ;
#17438 = CARTESIAN_POINT ( 'NONE',  ( 226.6211368133091923, 39.11482588413117867, -14.00000000000005507 ) ) ;
#17439 = VERTEX_POINT ( 'NONE', #12670 ) ;
#17440 = PLANE ( 'NONE',  #18682 ) ;
#17441 = DIRECTION ( 'NONE',  ( 0.8660254037844355990, 0.5000000000000054401, 0.000000000000000000 ) ) ;
#17442 = EDGE_CURVE ( 'NONE', #18235, #11211, #6330, .T. ) ;
#17443 = FACE_OUTER_BOUND ( 'NONE', #11313, .T. ) ;
#17444 = FACE_OUTER_BOUND ( 'NONE', #5279, .T. ) ;
#17445 = EDGE_CURVE ( 'NONE', #7667, #15787, #20709, .T. ) ;
#17446 = ORIENTED_EDGE ( 'NONE', *, *, #13273, .F. ) ;
#17447 = VERTEX_POINT ( 'NONE', #14165 ) ;
#17448 = LINE ( 'NONE', #1136, #8151 ) ;
#17449 = ORIENTED_EDGE ( 'NONE', *, *, #12890, .T. ) ;
#17450 = CONICAL_SURFACE ( 'NONE', #19144, 4.509097725792825528, 0.5235987755983015912 ) ;
#17451 = DIRECTION ( 'NONE',  ( -0.5000000000000051070, 0.8660254037844359321, -0.000000000000000000 ) ) ;
#17452 = DIRECTION ( 'NONE',  ( 0.5000000000000052180, -0.8660254037844355990, -1.665334536937734071E-16 ) ) ;
#17453 = DIRECTION ( 'NONE',  ( 0.000000000000000000, 0.000000000000000000, 1.000000000000000000 ) ) ;
#17454 = ADVANCED_FACE ( 'NONE', ( #2706 ), #15517, .F. ) ;
#17455 = DIRECTION ( 'NONE',  ( -1.060575238724903217E-16, -6.123233995736827666E-17, 1.000000000000000000 ) ) ;
#17456 = CARTESIAN_POINT ( 'NONE',  ( 214.2619155600624481, 14.99787291208556539, -20.59651891138172530 ) ) ;
#17457 = APPLICATION_CONTEXT ( 'automotive_design' ) ;
#17458 = ORIENTED_EDGE ( 'NONE', *, *, #3186, .T. ) ;
#17459 = CLOSED_SHELL ( 'NONE', ( #5864, #6688, #8507, #1450, #18083, #18342, #14484, #20544, #8687, #2531, #16681, #13131, #10370, #557, #19732 ) ) ;
#17460 = DIRECTION ( 'NONE',  ( -0.5000000000000047740, 0.8660254037844358210, 0.000000000000000000 ) ) ;
#17461 = ADVANCED_FACE ( 'NONE', ( #4392 ), #7561, .T. ) ;
#17462 = EDGE_LOOP ( 'NONE', ( #3627, #10062, #14827, #17897 ) ) ;
#17463 = CIRCLE ( 'NONE', #19154, 13.99999999999999822 ) ;
#17464 = FACE_OUTER_BOUND ( 'NONE', #11261, .T. ) ;
#17465 = CARTESIAN_POINT ( 'NONE',  ( 0.6679515277691319142, 50.95756615319989891, -7.179599708890708420 ) ) ;
#17466 = LINE ( 'NONE', #10883, #12318 ) ;
#17467 = AXIS2_PLACEMENT_3D ( 'NONE', #3816, #13266, #8475 ) ;
#17468 = EDGE_CURVE ( 'NONE', #9958, #14525, #1040, .T. ) ;
#17469 = CARTESIAN_POINT ( 'NONE',  ( 215.4747034159835550, 15.16702704537912183, -19.61257667712965258 ) ) ;
#17470 = CARTESIAN_POINT ( 'NONE',  ( -26.84899328648689476, 45.33011328186441347, -6.253688604731005185 ) ) ;
#17472 = EDGE_LOOP ( 'NONE', ( #15114, #7195, #18135, #6443 ) ) ;
#17471 = VERTEX_POINT ( 'NONE', #18919 ) ;
#17473 = ORIENTED_EDGE ( 'NONE', *, *, #1890, .F. ) ;
#17474 = DIRECTION ( 'NONE',  ( -0.6958540455341891695, 0.000000000000000000, 0.7181832268395738073 ) ) ;
#17475 = CARTESIAN_POINT ( 'NONE',  ( 199.2144802262915846, 21.04890371929339921, -14.00000000000005507 ) ) ;
#17476 = CARTESIAN_POINT ( 'NONE',  ( 228.4543736872085162, 38.69435111016120743, -10.51396113533826515 ) ) ;
#17477 = ORIENTED_EDGE ( 'NONE', *, *, #11199, .F. ) ;
#17478 = ORIENTED_EDGE ( 'NONE', *, *, #18305, .T. ) ;
#17479 = DIRECTION ( 'NONE',  ( -0.3878556453522086223, 0.6717856837524379676, -0.6310879443260591914 ) ) ;
#17480 = FACE_OUTER_BOUND ( 'NONE', #13307, .T. ) ;
#17481 = CARTESIAN_POINT ( 'NONE',  ( -10.57486132309840521, 50.32666072867165497, -15.61762382048297404 ) ) ;
#17482 = CIRCLE ( 'NONE', #18485, 5.000000000000002665 ) ;
#17483 = CARTESIAN_POINT ( 'NONE',  ( 4.000000000000000000, -3.518949890710766581, 4.553649124439118623E-15 ) ) ;
#17484 = VERTEX_POINT ( 'NONE', #7769 ) ;
#17485 = ORIENTED_EDGE ( 'NONE', *, *, #9772, .F. ) ;
#17486 = B_SPLINE_CURVE_WITH_KNOTS ( 'NONE', 3,
 ( #609, #13545, #510, #5565, #713, #3667, #12058, #6952, #5353, #2518, #11844, #8963, #18522, #6851, #18306, #3779, #10229, #16722, #19997, #5458 ),
 .UNSPECIFIED., .F., .F.,
 ( 4, 2, 2, 2, 2, 2, 2, 2, 2, 4 ),
 ( 0.03344032305337923255, 0.03481802353568227981, 0.03619572401798533401, 0.03895112498259143546, 0.04032882546489449660, 0.04170652594719755774, 0.04239537618834907790, 0.04308422642950059805, 0.04377307667065211821, 0.04446192691180363837 ),
 .UNSPECIFIED. ) ;
#17487 = CARTESIAN_POINT ( 'NONE',  ( -0.1767699604045824824, 65.74999999999997158, 2.481238266578629226 ) ) ;
#17488 = AXIS2_PLACEMENT_3D ( 'NONE', #935, #7278, #2845 ) ;
#17489 = DIRECTION ( 'NONE',  ( 0.5000000000000043299, -0.8660254037844361541, -1.401122807519728883E-16 ) ) ;
#17490 = CARTESIAN_POINT ( 'NONE',  ( 189.0579591095837202, 15.18503351853190608, -18.25196083293855054 ) ) ;
#17491 = CARTESIAN_POINT ( 'NONE',  ( 200.4973105777688431, 11.17487243767204852, -26.58724934764007486 ) ) ;
#17492 = CARTESIAN_POINT ( 'NONE',  ( 74.88379549237744470, 72.72378982140247672, -24.71895639200489825 ) ) ;
#17493 = DIRECTION ( 'NONE',  ( -0.5000000000000049960, 0.8660254037844357100, -0.000000000000000000 ) ) ;
#17494 = CARTESIAN_POINT ( 'NONE',  ( -28.65135327001111065, 64.04126923566909113, 2.490177094220571430 ) ) ;
#17495 = CARTESIAN_POINT ( 'NONE',  ( 216.7268875047958829, 8.998017661532479394, -6.310089745291985963 ) ) ;
#17496 = AXIS2_PLACEMENT_3D ( 'NONE', #3009, #20708, #15957 ) ;
#17497 = ORIENTED_EDGE ( 'NONE', *, *, #2209, .T. ) ;
#17498 = DIRECTION ( 'NONE',  ( 0.5000000000000051070, -0.8660254037844359321, 0.000000000000000000 ) ) ;
#17499 = DIRECTION ( 'NONE',  ( 0.7739085681710394793, 0.4468163201617139091, 0.4487991802004502873 ) ) ;
#17500 = CARTESIAN_POINT ( 'NONE',  ( -15.99999999999999289, 80.00000000000000000, 0.000000000000000000 ) ) ;
#17501 = CIRCLE ( 'NONE', #12078, 12.50000000000000000 ) ;
#17502 = ORIENTED_EDGE ( 'NONE', *, *, #7537, .F. ) ;
#17503 = CARTESIAN_POINT ( 'NONE',  ( 78.15559533904072964, 69.92979238318895341, 0.2890775442667399830 ) ) ;
#17504 = ORIENTED_EDGE ( 'NONE', *, *, #20931, .F. ) ;
#17505 = ORIENTED_EDGE ( 'NONE', *, *, #13250, .T. ) ;
#17506 = DIRECTION ( 'NONE',  ( -0.03412120668232990900, 0.05909966358935514474, -0.9976687691905399280 ) ) ;
#17507 = CARTESIAN_POINT ( 'NONE',  ( -28.99999999999999289, -10.00000000000000000, 15.00000000000000178 ) ) ;
#17508 = EDGE_CURVE ( 'NONE', #18381, #3402, #10847, .T. ) ;
#17509 = CARTESIAN_POINT ( 'NONE',  ( 205.8363079006329883, 14.25734397923043772, -1.053683606938506045 ) ) ;
#17510 = ORIENTED_EDGE ( 'NONE', *, *, #13551, .T. ) ;
#17511 = APPLICATION_PROTOCOL_DEFINITION ( 'draft international standard', 'automotive_design', 1998, #19600 ) ;
#17512 = CARTESIAN_POINT ( 'NONE',  ( 178.2433706042749009, 57.37193107572242923, -14.00000000000002842 ) ) ;
#17513 = ORIENTED_EDGE ( 'NONE', *, *, #337, .F. ) ;
#17514 = SURFACE_STYLE_USAGE ( .BOTH. , #4674 ) ;
#17515 = CARTESIAN_POINT ( 'NONE',  ( 30.00000000000000000, 0.000000000000000000, 28.99999999999999645 ) ) ;
#17516 = DIRECTION ( 'NONE',  ( -0.5000000000000051070, 0.8660254037844359321, -0.000000000000000000 ) ) ;
#17517 = DIRECTION ( 'NONE',  ( 0.8660254037844372643, 0.5000000000000027756, -0.000000000000000000 ) ) ;
#17518 = CARTESIAN_POINT ( 'NONE',  ( 26.00000000000000355, 0.000000000000000000, 4.171999999999999709 ) ) ;
#17519 = CARTESIAN_POINT ( 'NONE',  ( 220.2180084519553134, 35.41797800104779270, -14.00000000000005507 ) ) ;
#17520 = EDGE_CURVE ( 'NONE', #1291, #9961, #936, .T. ) ;
#17521 = PLANE ( 'NONE',  #2503 ) ;
#17522 = CARTESIAN_POINT ( 'NONE',  ( -14.99999999999999645, -10.00000000000000000, -28.99999999999999645 ) ) ;
#17523 = CARTESIAN_POINT ( 'NONE',  ( 220.0084750394892694, 33.64954575955419358, -9.992950739179644160 ) ) ;
#17524 = EDGE_LOOP ( 'NONE', ( #5322, #13406, #10753, #1578 ) ) ;
#17525 = DIRECTION ( 'NONE',  ( -0.8660254037844370423, -0.5000000000000026645, 0.000000000000000000 ) ) ;
#17526 = CARTESIAN_POINT ( 'NONE',  ( 81.62532777622794811, 56.02584323239422304, -1.826067817236490365 ) ) ;
#17527 = VECTOR ( 'NONE', #12616, 1000.000000000000114 ) ;
#17528 = DIRECTION ( 'NONE',  ( 0.5000000000000045519, -0.8660254037844360431, -4.006172263299080561E-16 ) ) ;
#17529 = CARTESIAN_POINT ( 'NONE',  ( 213.8661528393178060, 8.119191822981960627, -3.188775577416895324 ) ) ;
#17530 = ADVANCED_FACE ( 'NONE', ( #4185 ), #4601, .F. ) ;
#17532 = VERTEX_POINT ( 'NONE', #1428 ) ;
#17531 = ORIENTED_EDGE ( 'NONE', *, *, #10569, .F. ) ;
#17533 = ORIENTED_EDGE ( 'NONE', *, *, #17715, .F. ) ;
#17534 = EDGE_CURVE ( 'NONE', #16648, #12788, #9722, .T. ) ;
#17535 =( LENGTH_UNIT ( ) NAMED_UNIT ( * ) SI_UNIT ( .MILLI., .METRE. ) );
#17536 = DIRECTION ( 'NONE',  ( 0.5000000000000057732, -0.8660254037844353769, 0.000000000000000000 ) ) ;
#17537 = ORIENTED_EDGE ( 'NONE', *, *, #6267, .T. ) ;
#17538 = CARTESIAN_POINT ( 'NONE',  ( -27.87293505806218619, 79.99999999978210496, -3.927153389733302191 ) ) ;
#17539 = DIRECTION ( 'NONE',  ( 0.000000000000000000, 0.000000000000000000, 1.000000000000000000 ) ) ;
#17540 = ORIENTED_EDGE ( 'NONE', *, *, #9117, .F. ) ;
#17541 = VECTOR ( 'NONE', #12357, 1000.000000000000114 ) ;
#17542 = PLANE ( 'NONE',  #9534 ) ;
#17543 = SHAPE_REPRESENTATION_RELATIONSHIP ( 'NONE' , 'NONE' ,  #9759, #7549 ) ;
#17544 = AXIS2_PLACEMENT_3D ( 'NONE', #18554, #7511, #20135 ) ;
#17545 = VERTEX_POINT ( 'NONE', #10965 ) ;
#17546 = CYLINDRICAL_SURFACE ( 'NONE', #12938, 3.902363844300889451 ) ;
#17547 = DIRECTION ( 'NONE',  ( 0.7951984747223626027, 0.4591080534401424385, 0.3960797660391544017 ) ) ;
#17548 = EDGE_CURVE ( 'NONE', #8656, #681, #7349, .T. ) ;
#17549 = EDGE_CURVE ( 'NONE', #122, #11547, #5750, .T. ) ;
#17550 = CARTESIAN_POINT ( 'NONE',  ( 219.1096994420543922, 36.51014630340509370, -14.00000000000005507 ) ) ;
#17551 = CARTESIAN_POINT ( 'NONE',  ( 221.8782118065657869, 32.54242143996614089, -11.94979443502200844 ) ) ;
#17552 = ORIENTED_EDGE ( 'NONE', *, *, #1106, .T. ) ;
#17553 = CARTESIAN_POINT ( 'NONE',  ( 32.36389338619004263, 157.9004617752989930, -12.50000000000000000 ) ) ;
#17554 = EDGE_CURVE ( 'NONE', #11821, #19224, #19990, .T. ) ;
#17555 = EDGE_LOOP ( 'NONE', ( #16427, #1052, #20379, #3567, #19818, #13832, #232 ) ) ;
#17556 = ORIENTED_EDGE ( 'NONE', *, *, #3079, .T. ) ;
#17557 = AXIS2_PLACEMENT_3D ( 'NONE', #6353, #17726, #19203 ) ;
#17558 = CARTESIAN_POINT ( 'NONE',  ( 208.8107687779841228, 4.427644383670616079, -14.00000000000005507 ) ) ;
#17559 = CARTESIAN_POINT ( 'NONE',  ( 205.0042238655992719, 9.652942120212628652, -25.96516918080906677 ) ) ;
#17560 = DIRECTION ( 'NONE',  ( 0.000000000000000000, -0.000000000000000000, -1.000000000000000000 ) ) ;
#17561 = EDGE_CURVE ( 'NONE', #2300, #16434, #8381, .T. ) ;
#17562 = DIRECTION ( 'NONE',  ( 0.5000000000000045519, -0.8660254037844361541, 0.000000000000000000 ) ) ;
#17563 = DIRECTION ( 'NONE',  ( 0.8528685319524385022, 0.4924038765061083955, -0.1736481776669415444 ) ) ;
#17564 = ORIENTED_EDGE ( 'NONE', *, *, #12522, .F. ) ;
#17565 = EDGE_CURVE ( 'NONE', #5172, #3434, #19232, .T. ) ;
#17566 = DIRECTION ( 'NONE',  ( 0.8660254037844370423, 0.5000000000000026645, -0.000000000000000000 ) ) ;
#17567 = AXIS2_PLACEMENT_3D ( 'NONE', #13621, #15332, #14044 ) ;
#17568 = EDGE_LOOP ( 'NONE', ( #3001, #4426, #8278, #18254 ) ) ;
#17569 = PLANE ( 'NONE',  #14661 ) ;
#17570 = CARTESIAN_POINT ( 'NONE',  ( -6.040070365067144564, 50.06279613334914558, -13.94107049437905665 ) ) ;
#17571 = DIRECTION ( 'NONE',  ( 0.000000000000000000, -1.000000000000000000, 0.000000000000000000 ) ) ;
#17572 = EDGE_CURVE ( 'NONE', #15887, #3796, #4699, .T. ) ;
#17573 = CARTESIAN_POINT ( 'NONE',  ( 199.6867264275208527, -0.3249176845898890664, -20.75355104716098964 ) ) ;
#17574 = CARTESIAN_POINT ( 'NONE',  ( -15.99999999999998934, 45.63508326896292289, -12.50000000000000000 ) ) ;
#17576 = VERTEX_POINT ( 'NONE', #5105 ) ;
#17575 = ORIENTED_EDGE ( 'NONE', *, *, #7891, .T. ) ;
#17577 = DIRECTION ( 'NONE',  ( 0.8660254037844354880, 0.5000000000000053291, 0.000000000000000000 ) ) ;
#17578 = DIRECTION ( 'NONE',  ( -0.8660254037844361541, -0.5000000000000045519, -4.336808689942050770E-16 ) ) ;
#17579 = ADVANCED_FACE ( 'NONE', ( #14689 ), #145, .T. ) ;
#17580 = ORIENTED_EDGE ( 'NONE', *, *, #19118, .F. ) ;
#17581 = ORIENTED_EDGE ( 'NONE', *, *, #18057, .T. ) ;
#17582 = CARTESIAN_POINT ( 'NONE',  ( 216.7381715613988433, 9.262131738456792718, -6.204501730076263932 ) ) ;
#17583 = DIRECTION ( 'NONE',  ( 0.8660254037844368202, 0.5000000000000031086, -1.942890293094023946E-16 ) ) ;
#17584 = DIRECTION ( 'NONE',  ( -0.8660254037844355990, -0.5000000000000054401, -1.334965637238773043E-14 ) ) ;
#17585 = EDGE_CURVE ( 'NONE', #5345, #3315, #20236, .T. ) ;
#17586 = DIRECTION ( 'NONE',  ( -0.8137976813493725814, -0.4698463103929604867, -0.3420201433256626622 ) ) ;
#17587 = EDGE_LOOP ( 'NONE', ( #11131, #11687, #1236, #9512, #502, #7502 ) ) ;
#17588 = CIRCLE ( 'NONE', #19930, 3.619616396367202782 ) ;
#17589 = ORIENTED_EDGE ( 'NONE', *, *, #1655, .F. ) ;
#17590 = DIRECTION ( 'NONE',  ( -0.5566703992264184775, -0.3213938048432735117, -0.7660444431189770143 ) ) ;
#17591 = EDGE_CURVE ( 'NONE', #5809, #5880, #3285, .T. ) ;
#17592 = LINE ( 'NONE', #6328, #20239 ) ;
#17593 = EDGE_CURVE ( 'NONE', #18887, #844, #8183, .T. ) ;
#17594 = CARTESIAN_POINT ( 'NONE',  ( 221.4355490342864812, 33.10315778620316962, -16.74850582525162679 ) ) ;
#17595 = ADVANCED_FACE ( 'NONE', ( #1531 ), #19526, .F. ) ;
#17596 = CARTESIAN_POINT ( 'NONE',  ( 228.3892714728390843, 39.13358052910029272, -18.16400186620062485 ) ) ;
#17597 = CARTESIAN_POINT ( 'NONE',  ( -31.81189201763190511, 64.84542049530487873, 2.499203484743047099 ) ) ;
#17598 = DIRECTION ( 'NONE',  ( 0.8660254037844375974, 0.5000000000000019984, 0.000000000000000000 ) ) ;
#17599 = MANIFOLD_SOLID_BREP ( 'Cut-Extrude6', #5572 ) ;
#17600 = EDGE_CURVE ( 'NONE', #11033, #2878, #1629, .T. ) ;
#17601 = CARTESIAN_POINT ( 'NONE',  ( 217.5692528822465306, 9.484357538959612199, -5.585956497640099272 ) ) ;
#17602 = CARTESIAN_POINT ( 'NONE',  ( 42.30949999999999989, 0.000000000000000000, 0.000000000000000000 ) ) ;
#17603 = DIRECTION ( 'NONE',  ( -0.5000000000000049960, 0.8660254037844358210, 0.000000000000000000 ) ) ;
#17604 = VECTOR ( 'NONE', #11824, 1000.000000000000227 ) ;
#17605 = EDGE_LOOP ( 'NONE', ( #1371, #19877, #10757, #650 ) ) ;
#17606 = AXIS2_PLACEMENT_3D ( 'NONE', #20721, #17759, #7885 ) ;
#17607 = CARTESIAN_POINT ( 'NONE',  ( 82.90420097239591257, 63.09545557312737429, 0.5024926129020395038 ) ) ;
#17608 = VECTOR ( 'NONE', #12598, 1000.000000000000114 ) ;
#17609 = ORIENTED_EDGE ( 'NONE', *, *, #14894, .T. ) ;
#17610 = ORIENTED_EDGE ( 'NONE', *, *, #12022, .F. ) ;
#17611 = CARTESIAN_POINT ( 'NONE',  ( 1.484819526751601559, 76.25000000000000000, -2.578432583507792586 ) ) ;
#17612 = ADVANCED_FACE ( 'NONE', ( #4804 ), #42, .F. ) ;
#17613 = VECTOR ( 'NONE', #9760, 1000.000000000000227 ) ;
#17614 = CARTESIAN_POINT ( 'NONE',  ( 202.3258709495397625, 22.84526599091486077, -25.94618751764496878 ) ) ;
#17615 = APPLICATION_PROTOCOL_DEFINITION ( 'draft international standard', 'automotive_design', 1998, #14501 ) ;
#17616 = DIRECTION ( 'NONE',  ( -0.8660254037844362651, -0.5000000000000043299, 0.000000000000000000 ) ) ;
#17617 = EDGE_LOOP ( 'NONE', ( #18107, #18569, #14948, #9952 ) ) ;
#17618 = DIRECTION ( 'NONE',  ( 0.000000000000000000, 1.000000000000000000, -1.294035738186424998E-16 ) ) ;
#17619 = FACE_OUTER_BOUND ( 'NONE', #1947, .T. ) ;
#17620 = CARTESIAN_POINT ( 'NONE',  ( 0.000000000000000000, -2.342598717236899386, 4.057500000000001883 ) ) ;
#17621 = CARTESIAN_POINT ( 'NONE',  ( 199.2144802262915846, 21.04890371929339921, -14.00000000000005507 ) ) ;
#17622 = VECTOR ( 'NONE', #4196, 1000.000000000000000 ) ;
#17623 = FACE_OUTER_BOUND ( 'NONE', #5759, .T. ) ;
#17624 = LINE ( 'NONE', #3300, #9214 ) ;
#17625 = CARTESIAN_POINT ( 'NONE',  ( 229.7418667850695613, 36.79081672623772903, -13.95097276009443732 ) ) ;
#17626 = CARTESIAN_POINT ( 'NONE',  ( 216.6737232845935068, 8.967323284687328311, -21.59012016402729728 ) ) ;
#17627 = LINE ( 'NONE', #15939, #12914 ) ;
#17628 = DIRECTION ( 'NONE',  ( 0.000000000000000000, 0.000000000000000000, -1.000000000000000000 ) ) ;
#17629 = EDGE_LOOP ( 'NONE', ( #17449, #12242, #12847, #3611 ) ) ;
#17630 = CARTESIAN_POINT ( 'NONE',  ( 195.4150569263803732, 4.116634006550261127, -12.64773574313024440 ) ) ;
#17631 = CARTESIAN_POINT ( 'NONE',  ( 59.42304552939003770, 84.84901963477547326, -9.175363098692354669 ) ) ;
#17632 = CIRCLE ( 'NONE', #5075, 10.26794919243111437 ) ;
#17633 = CARTESIAN_POINT ( 'NONE',  ( 44.01452848080091229, 187.7209698509878137, 11.00000000000001066 ) ) ;
#17634 = CIRCLE ( 'NONE', #4100, 5.000000000000002665 ) ;
#17635 = CARTESIAN_POINT ( 'NONE',  ( 5.000000000000004441, 0.000000000000000000, 0.000000000000000000 ) ) ;
#17637 = VERTEX_POINT ( 'NONE', #14378 ) ;
#17636 = ORIENTED_EDGE ( 'NONE', *, *, #13282, .F. ) ;
#17638 = ORIENTED_EDGE ( 'NONE', *, *, #20680, .F. ) ;
#17639 = PLANE ( 'NONE',  #16317 ) ;
#17640 = UNCERTAINTY_MEASURE_WITH_UNIT (LENGTH_MEASURE( 1.000000000000000082E-05 ), #13415, 'distance_accuracy_value', 'NONE');
#17641 = ORIENTED_EDGE ( 'NONE', *, *, #20728, .F. ) ;
#17642 = VECTOR ( 'NONE', #17902, 1000.000000000000000 ) ;
#17643 = DIRECTION ( 'NONE',  ( 0.8660254037844355990, 0.5000000000000054401, 0.000000000000000000 ) ) ;
#17644 = ORIENTED_EDGE ( 'NONE', *, *, #8234, .F. ) ;
#17645 = DIRECTION ( 'NONE',  ( 0.8660254037844380415, 0.5000000000000014433, 0.000000000000000000 ) ) ;
#17646 = EDGE_CURVE ( 'NONE', #11719, #5880, #3321, .T. ) ;
#17647 = CARTESIAN_POINT ( 'NONE',  ( -29.18969730202500301, 79.49366880382837053, -8.593311550915920805 ) ) ;
#17648 = DIRECTION ( 'NONE',  ( -0.5000000000000045519, 0.8660254037844361541, 0.000000000000000000 ) ) ;
#17649 = CONICAL_SURFACE ( 'NONE', #15960, 10.85470691220533190, 0.8171114040043576665 ) ;
#17650 = ORIENTED_EDGE ( 'NONE', *, *, #6938, .F. ) ;
#17651 =( BOUNDED_SURFACE ( )  B_SPLINE_SURFACE ( 3, 2, ( 
 ( #9896, #167, #6128 ),
 ( #16486, #17883, #11619 ),
 ( #11022, #18081, #9796 ),
 ( #11404, #19552, #14610 ),
 ( #19082, #1969, #6023 ),
 ( #13006, #16188, #4555 ),
 ( #8207, #5029, #11505 ),
 ( #5133, #2867, #17492 ),
 ( #16392, #1657, #20550 ),
 ( #3549, #16285, #8096 ),
 ( #1762, #19449, #10915 ),
 ( #4928, #1865, #3345 ),
 ( #6611, #17984, #3448 ),
 ( #14819, #268, #4452 ),
 ( #6713, #19660, #9991 ),
 ( #14118, #12512, #17386 ),
 ( #690, #800, #7146 ),
 ( #15345, #16906, #3649 ),
 ( #588, #3760, #19971 ),
 ( #8636, #8533, #10535 ),
 ( #2079, #13635, #8846 ),
 ( #5438, #16590, #20087 ),
 ( #16806, #2285, #18503 ),
 ( #10425, #5333, #6931 ),
 ( #18184, #6835, #5652 ),
 ( #13523, #15033, #12142 ),
 ( #2387, #8740, #18604 ),
 ( #18284, #383, #492 ),
 ( #11937, #19766, #11823 ),
 ( #5230, #4078, #10316 ),
 ( #10212, #11721, #16705 ),
 ( #18396, #3975, #2184 ),
 ( #15134, #13418, #5549 ),
 ( #10102, #12039, #19866 ),
 ( #7252, #13318, #20189 ),
 ( #14916, #13735, #17020 ),
 ( #8416, #7041, #3865 ),
 ( #15238, #15096, #10067 ),
 ( #342, #11470, #5196 ),
 ( #6575, #4993, #4899 ),
 ( #3716, #14783, #19420 ),
 ( #8273, #137, #6788 ),
 ( #16449, #11370, #16356 ),
 ( #18048, #16558, #14885 ),
 ( #8491, #19515, #19619 ),
 ( #8598, #14995, #551 ),
 ( #17845, #452, #6678 ),
 ( #3409, #6898, #13279 ),
 ( #19724, #1725, #13378 ),
 ( #18148, #5297, #11683 ),
 ( #12973, #9761, #237 ),
 ( #3615, #11578, #19829 ),
 ( #1829, #3312, #16245 ),
 ( #5096, #8174, #13174 ),
 ( #9957, #2038, #3516 ),
 ( #14683, #11789, #13074 ),
 ( #17946, #18252, #1936 ),
 ( #9861, #10171, #16666 ),
 ( #8383, #2147, #13599 ),
 ( #12102, #12004, #13489 ),
 ( #2249, #973, #5402 ),
 ( #13804, #7109, #15615 ),
 ( #10489, #4259, #2353 ),
 ( #10711, #2464, #18571 ) ),
 .UNSPECIFIED., .F., .F., .F. ) 
 B_SPLINE_SURFACE_WITH_KNOTS ( ( 4, 2, 2, 2, 2, 2, 2, 2, 2, 2, 2, 2, 2, 2, 2, 2, 2, 2, 2, 2, 2, 2, 2, 2, 2, 2, 2, 2, 2, 2, 2, 4 ),
 ( 3, 3 ),
 ( 0.000000000000000000, 0.004303368843509257358, 0.008606737687018514715, 0.01291010653052777207, 0.01721347537403702943, 0.01936515979579165811, 0.02151684421754628679, 0.02366852863930091547, 0.02474437085017822807, 0.02582021306105554415, 0.02689605527193286022, 0.02797189748281017282, 0.02904773969368748543, 0.03012358190456480150, 0.03227526632631942671, 0.03442695074807405886, 0.03657863516982869101, 0.03873031959158331622, 0.04088200401333794143, 0.04303368843509257358, 0.04733705727860183093, 0.04841289948947914701, 0.04948874170035645614, 0.05164042612211108829, 0.05379211054386572044, 0.05594379496562034565, 0.05809547938737497086, 0.05917132159825228693, 0.06024716380912960301, 0.06455053265263885343, 0.06670221707439348557, 0.06885390149614811772 ),
 ( 0.000000000000000000, 1.000000000000000000 ),
 .UNSPECIFIED. ) 
 GEOMETRIC_REPRESENTATION_ITEM ( )  RATIONAL_B_SPLINE_SURFACE ( (
 ( 1.000000000000000000, 0.7477234448260038358, 1.000000000000000000),
 ( 1.000000000000000000, 0.7740357663989568815, 1.000000000000000000),
 ( 1.000000000000000000, 0.7979944444720340480, 1.000000000000000000),
 ( 1.000000000000000000, 0.8415418573160285964, 1.000000000000000000),
 ( 1.000000000000000000, 0.8611354141022936615, 1.000000000000000000),
 ( 1.000000000000000000, 0.8962784209894617549, 1.000000000000000000),
 ( 1.000000000000000000, 0.9118336320813347218, 1.000000000000000000),
 ( 1.000000000000000000, 0.9390903228898979105, 1.000000000000000000),
 ( 1.000000000000000000, 0.9507059349589174202, 1.000000000000000000),
 ( 1.000000000000000000, 0.9652792442033365505, 1.000000000000000000),
 ( 1.000000000000000000, 0.9696658626168446204, 1.000000000000000000),
 ( 1.000000000000000000, 0.9774477440020008512, 1.000000000000000000),
 ( 1.000000000000000000, 0.9808482499402014776, 1.000000000000000000),
 ( 1.000000000000000000, 0.9866388090191381410, 1.000000000000000000),
 ( 1.000000000000000000, 0.9890362374316506999, 1.000000000000000000),
 ( 1.000000000000000000, 0.9917478669874124630, 1.000000000000000000),
 ( 1.000000000000000000, 0.9925034521094587836, 1.000000000000000000),
 ( 1.000000000000000000, 0.9936052247524241876, 1.000000000000000000),
 ( 1.000000000000000000, 0.9939601189669974302, 1.000000000000000000),
 ( 1.000000000000000000, 0.9942187593714609806, 1.000000000000000000),
 ( 1.000000000000000000, 0.9941154017096719420, 1.000000000000000000),
 ( 1.000000000000000000, 0.9934872688014458886, 1.000000000000000000),
 ( 1.000000000000000000, 0.9929544046041767213, 1.000000000000000000),
 ( 1.000000000000000000, 0.9915541073466924704, 1.000000000000000000),
 ( 1.000000000000000000, 0.9906898267772793476, 1.000000000000000000),
 ( 1.000000000000000000, 0.9886839553106602230, 1.000000000000000000),
 ( 1.000000000000000000, 0.9875405405517138080, 1.000000000000000000),
 ( 1.000000000000000000, 0.9837407462627784094, 1.000000000000000000),
 ( 1.000000000000000000, 0.9807661871025340483, 1.000000000000000000),
 ( 1.000000000000000000, 0.9740929453405124949, 1.000000000000000000),
 ( 1.000000000000000000, 0.9703914076251105580, 1.000000000000000000),
 ( 1.000000000000000000, 0.9623642252138717712, 1.000000000000000000),
 ( 1.000000000000000000, 0.9580128855153311473, 1.000000000000000000),
 ( 1.000000000000000000, 0.9489407451290137185, 1.000000000000000000),
 ( 1.000000000000000000, 0.9442201479404100928, 1.000000000000000000),
 ( 1.000000000000000000, 0.9345645691926910414, 1.000000000000000000),
 ( 1.000000000000000000, 0.9296290518281515869, 1.000000000000000000),
 ( 1.000000000000000000, 0.9197163133202026497, 1.000000000000000000),
 ( 1.000000000000000000, 0.9147061918368204481, 1.000000000000000000),
 ( 1.000000000000000000, 0.9002701591943753634, 1.000000000000000000),
 ( 1.000000000000000000, 0.8913752732212651964, 1.000000000000000000),
 ( 1.000000000000000000, 0.8822678195319330063, 1.000000000000000000),
 ( 1.000000000000000000, 0.8805477477376374429, 1.000000000000000000),
 ( 1.000000000000000000, 0.8773422126919282471, 1.000000000000000000),
 ( 1.000000000000000000, 0.8758553697949494898, 1.000000000000000000),
 ( 1.000000000000000000, 0.8718595913002757936, 1.000000000000000000),
 ( 1.000000000000000000, 0.8697876269511248815, 1.000000000000000000),
 ( 1.000000000000000000, 0.8669277261913932442, 1.000000000000000000),
 ( 1.000000000000000000, 0.8661397616582809933, 1.000000000000000000),
 ( 1.000000000000000000, 0.8659341656688209765, 1.000000000000000000),
 ( 1.000000000000000000, 0.8665328086759263027, 1.000000000000000000),
 ( 1.000000000000000000, 0.8690449782978997284, 1.000000000000000000),
 ( 1.000000000000000000, 0.8709515724093638278, 1.000000000000000000),
 ( 1.000000000000000000, 0.8746833890562724090, 1.000000000000000000),
 ( 1.000000000000000000, 0.8760725967190144958, 1.000000000000000000),
 ( 1.000000000000000000, 0.8791235325893823616, 1.000000000000000000),
 ( 1.000000000000000000, 0.8807908387558892604, 1.000000000000000000),
 ( 1.000000000000000000, 0.8896941911137391523, 1.000000000000000000),
 ( 1.000000000000000000, 0.8985060072108992379, 1.000000000000000000),
 ( 1.000000000000000000, 0.9128644761645609007, 1.000000000000000000),
 ( 1.000000000000000000, 0.9178532540556407771, 1.000000000000000000),
 ( 1.000000000000000000, 0.9277720463150811447, 1.000000000000000000),
 ( 1.000000000000000000, 0.9327312656600242891, 1.000000000000000000),
 ( 1.000000000000000000, 0.9375990638454466675, 1.000000000000000000) ) ) 
 REPRESENTATION_ITEM ( '' )  SURFACE ( )  );
#17652 = DIRECTION ( 'NONE',  ( 0.6946590618905410519, 0.4010615963775224224, -0.5971585917027962820 ) ) ;
#17653 = TOROIDAL_SURFACE ( 'NONE', #15637, 6.500000000000000888, 1.500000000000000000 ) ;
#17654 = CIRCLE ( 'NONE', #8490, 7.155882939242646401 ) ;
#17655 = AXIS2_PLACEMENT_3D ( 'NONE', #15766, #18831, #9367 ) ;
#17656 = ORIENTED_EDGE ( 'NONE', *, *, #9514, .F. ) ;
#17657 = CARTESIAN_POINT ( 'NONE',  ( 210.5263754848605231, 5.675749601516248077, -25.93669565428271184 ) ) ;
#17658 = ADVANCED_FACE ( 'NONE', ( #10389 ), #11906, .F. ) ;
#17659 = DIRECTION ( 'NONE',  ( -0.5000000000000045519, 0.8660254037844361541, 0.000000000000000000 ) ) ;
#17660 = ORIENTED_EDGE ( 'NONE', *, *, #20779, .F. ) ;
#17661 = VECTOR ( 'NONE', #3160, 1000.000000000000227 ) ;
#17662 = DIRECTION ( 'NONE',  ( -0.8660254037844360431, -0.5000000000000045519, -4.336808689942050277E-16 ) ) ;
#17663 = ORIENTED_EDGE ( 'NONE', *, *, #2587, .T. ) ;
#17664 = CARTESIAN_POINT ( 'NONE',  ( 30.10683012259193703, -10.00000000000000000, 4.999999999999997335 ) ) ;
#17665 = CIRCLE ( 'NONE', #11230, 11.94520687646042667 ) ;
#17666 = VERTEX_POINT ( 'NONE', #3623 ) ;
#17667 = CARTESIAN_POINT ( 'NONE',  ( 197.0455819868763570, 9.182016006550787424, -24.58554911381517627 ) ) ;
#17668 = CARTESIAN_POINT ( 'NONE',  ( 218.3963147110919749, 38.36726605008328761, -15.54214587067326292 ) ) ;
#17669 = LINE ( 'NONE', #7894, #14140 ) ;
#17670 = EDGE_CURVE ( 'NONE', #9756, #4589, #7375, .T. ) ;
#17671 = VECTOR ( 'NONE', #16421, 1000.000000000000114 ) ;
#17672 = DIRECTION ( 'NONE',  ( 0.000000000000000000, 0.000000000000000000, 1.000000000000000000 ) ) ;
#17673 = CARTESIAN_POINT ( 'NONE',  ( 4.000000000000000000, -2.639212418033078045, -1.523749999999994831 ) ) ;
#17674 = ORIENTED_EDGE ( 'NONE', *, *, #7678, .F. ) ;
#17675 = FACE_OUTER_BOUND ( 'NONE', #5632, .T. ) ;
#17676 = EDGE_CURVE ( 'NONE', #5808, #19064, #6052, .T. ) ;
#17677 = EDGE_CURVE ( 'NONE', #4969, #423, #2656, .T. ) ;
#17678 = CARTESIAN_POINT ( 'NONE',  ( 1.114207876027680122, 51.53275387072061875, -5.884738422014940795 ) ) ;
#17679 = DIRECTION ( 'NONE',  ( -1.000000000000000000, 0.000000000000000000, -0.000000000000000000 ) ) ;
#17680 = CIRCLE ( 'NONE', #16333, 7.155882939242646401 ) ;
#17681 = DIRECTION ( 'NONE',  ( 0.8660254037844377084, 0.5000000000000015543, 0.000000000000000000 ) ) ;
#17682 = VECTOR ( 'NONE', #2112, 1000.000000000000000 ) ;
#17683 = CARTESIAN_POINT ( 'NONE',  ( -17.53792359058950723, 45.60860274098917699, -12.42895697958611123 ) ) ;
#17685 = VERTEX_POINT ( 'NONE', #7010 ) ;
#17684 = ORIENTED_EDGE ( 'NONE', *, *, #15750, .F. ) ;
#17686 = ORIENTED_EDGE ( 'NONE', *, *, #3179, .T. ) ;
#17687 = LINE ( 'NONE', #4538, #9482 ) ;
#17688 = DIRECTION ( 'NONE',  ( -0.8660254037844355990, -0.5000000000000054401, 1.070753688201932557E-14 ) ) ;
#17689 = CARTESIAN_POINT ( 'NONE',  ( -4.382345773779359632, 80.00000000021817925, -4.628091497300713009 ) ) ;
#17690 = EDGE_LOOP ( 'NONE', ( #14162, #7772, #3497, #8224 ) ) ;
#17691 = EDGE_CURVE ( 'NONE', #504, #3051, #15866, .T. ) ;
#17692 = CARTESIAN_POINT ( 'NONE',  ( -16.00000000000007105, 58.38562172233837089, -4.999999999999997335 ) ) ;
#17693 = CARTESIAN_POINT ( 'NONE',  ( 211.6737232845934500, 17.62757732253168541, -21.59012016402730083 ) ) ;
#17694 = CARTESIAN_POINT ( 'NONE',  ( 7.999999999999998224, 0.000000000000000000, -4.400000000000000355 ) ) ;
#17695 = ORIENTED_EDGE ( 'NONE', *, *, #14716, .F. ) ;
#17696 = EDGE_LOOP ( 'NONE', ( #1577, #2973 ) ) ;
#17697 = DIRECTION ( 'NONE',  ( 0.000000000000000000, 0.000000000000000000, -1.000000000000000000 ) ) ;
#17698 = ORIENTED_EDGE ( 'NONE', *, *, #10967, .T. ) ;
#17699 = AXIS2_PLACEMENT_3D ( 'NONE', #13505, #12118, #19950 ) ;
#17700 = AXIS2_PLACEMENT_3D ( 'NONE', #4028, #20242, #18664 ) ;
#17701 = EDGE_CURVE ( 'NONE', #2297, #18411, #6309, .T. ) ;
#17702 = SHAPE_REPRESENTATION_RELATIONSHIP ( 'NONE' , 'NONE' ,  #6911, #2499 ) ;
#17703 = VECTOR ( 'NONE', #3241, 1000.000000000000227 ) ;
#17704 = CARTESIAN_POINT ( 'NONE',  ( -11.00000000000000355, 15.43320684789191333, 11.45643923738960446 ) ) ;
#17705 = EDGE_CURVE ( 'NONE', #17269, #9496, #15624, .T. ) ;
#17706 = CARTESIAN_POINT ( 'NONE',  ( 197.6726970570908293, -1.230104231997219300, -14.01558723443171850 ) ) ;
#17707 = CARTESIAN_POINT ( 'NONE',  ( -31.95547536107751796, 62.33962363497189330, 2.266630807618284393 ) ) ;
#17708 = DIRECTION ( 'NONE',  ( -0.8660254037844378194, -0.5000000000000013323, -0.000000000000000000 ) ) ;
#17709 = DIRECTION ( 'NONE',  ( 0.5000000000000054401, -0.8660254037844354880, 0.000000000000000000 ) ) ;
#17710 = DIRECTION ( 'NONE',  ( 1.000000000000000000, -0.000000000000000000, -0.000000000000000000 ) ) ;
#17711 = LINE ( 'NONE', #4762, #1062 ) ;
#17712 = ORIENTED_EDGE ( 'NONE', *, *, #20067, .T. ) ;
#17713 = CONICAL_SURFACE ( 'NONE', #4161, 10.85470691220533190, 0.8171114040043576665 ) ;
#17714 = CARTESIAN_POINT ( 'NONE',  ( 68.09635467782193530, 74.89565063689929048, -3.661860698923952384 ) ) ;
#17715 = EDGE_CURVE ( 'NONE', #13875, #38, #4366, .T. ) ;
#17716 = VERTEX_POINT ( 'NONE', #18998 ) ;
#17717 = EDGE_CURVE ( 'NONE', #2773, #15199, #4476, .T. ) ;
#17718 = ORIENTED_EDGE ( 'NONE', *, *, #17561, .T. ) ;
#17719 = CARTESIAN_POINT ( 'NONE',  ( 0.9726465904711251165, 73.17878816827938238, 0.08443632836958642196 ) ) ;
#17720 = DIRECTION ( 'NONE',  ( -0.5000000000000049960, 0.8660254037844358210, -0.000000000000000000 ) ) ;
#17721 = CARTESIAN_POINT ( 'NONE',  ( 10.49211908931699178, 5.000000000000000000, 5.000000000000000000 ) ) ;
#17722 = SHAPE_DEFINITION_REPRESENTATION ( #13299, #6230 ) ;
#17723 = ADVANCED_FACE ( 'NONE', ( #5937 ), #18788, .F. ) ;
#17724 = DIRECTION ( 'NONE',  ( -0.5000000000000034417, 0.000000000000000000, 0.8660254037844367092 ) ) ;
#17725 = ORIENTED_EDGE ( 'NONE', *, *, #10434, .T. ) ;
#17726 = DIRECTION ( 'NONE',  ( -0.5000000000000054401, 0.8660254037844354880, -0.000000000000000000 ) ) ;
#17727 = DIRECTION ( 'NONE',  ( -0.5000000000000051070, 0.8660254037844359321, -0.000000000000000000 ) ) ;
#17728 = CIRCLE ( 'NONE', #16374, 5.000000000000000000 ) ;
#17729 = CARTESIAN_POINT ( 'NONE',  ( 210.8238100345766384, 28.21933447757778168, -15.99832059698782061 ) ) ;
#17730 = DIRECTION ( 'NONE',  ( -0.5000000000000045519, 0.8660254037844361541, 4.006172263299079574E-16 ) ) ;
#17731 = PLANE ( 'NONE',  #14089 ) ;
#17732 = DIRECTION ( 'NONE',  ( 0.000000000000000000, -0.7775157341892985352, 0.6288634852558033783 ) ) ;
#17733 = B_SPLINE_CURVE_WITH_KNOTS ( 'NONE', 3,
 ( #13715, #13927, #5311, #9128 ),
 .UNSPECIFIED., .F., .F.,
 ( 4, 4 ),
 ( 2.140854117600596434E-05, 0.0005873347634711240063 ),
 .UNSPECIFIED. ) ;
#17734 = ADVANCED_FACE ( 'NONE', ( #7643 ), #17302, .F. ) ;
#17735 = DIRECTION ( 'NONE',  ( 0.5000000000000044409, -0.8660254037844360431, 0.000000000000000000 ) ) ;
#17736 = FACE_OUTER_BOUND ( 'NONE', #1766, .T. ) ;
#17737 = DIRECTION ( 'NONE',  ( -0.5000000000000047740, 0.8660254037844358210, 0.000000000000000000 ) ) ;
#17738 = EDGE_LOOP ( 'NONE', ( #13120, #7576, #4799, #4254 ) ) ;
#17739 = FACE_BOUND ( 'NONE', #17696, .T. ) ;
#17740 = CARTESIAN_POINT ( 'NONE',  ( 82.80355713680948782, 63.70540732580594323, 0.5609838852837873979 ) ) ;
#17741 = MANIFOLD_SOLID_BREP ( 'Chamfer3', #16775 ) ;
#17742 = CARTESIAN_POINT ( 'NONE',  ( 220.7798625593474924, 34.23884007463320955, -10.43783272703044673 ) ) ;
#17743 = AXIS2_PLACEMENT_3D ( 'NONE', #5385, #534, #320 ) ;
#17744 = CARTESIAN_POINT ( 'NONE',  ( 202.0139385235187035, 1.276312697262135920, -4.003039906353937916 ) ) ;
#17745 = CIRCLE ( 'NONE', #3848, 4.730184897849355252 ) ;
#17747 = ORIENTED_EDGE ( 'NONE', *, *, #13268, .F. ) ;
#17746 = ORIENTED_EDGE ( 'NONE', *, *, #9644, .F. ) ;
#17748 = ORIENTED_EDGE ( 'NONE', *, *, #18084, .T. ) ;
#17749 = CARTESIAN_POINT ( 'NONE',  ( 219.7263601677211966, 36.06355974282531918, -17.70629034850377082 ) ) ;
#17750 = ORIENTED_EDGE ( 'NONE', *, *, #9970, .T. ) ;
#17751 = CARTESIAN_POINT ( 'NONE',  ( -27.18818224385167426, 79.75568800831801752, -9.793444445059897419 ) ) ;
#17752 = CARTESIAN_POINT ( 'NONE',  ( 219.0491705959332478, 37.23648648751787960, -17.11800046810210674 ) ) ;
#17753 = DIRECTION ( 'NONE',  ( 0.2300325188655767683, -0.3984280100682212056, 0.8878852184023763305 ) ) ;
#17754 = AXIS2_PLACEMENT_3D ( 'NONE', #7143, #13315, #489 ) ;
#17755 = B_SPLINE_CURVE_WITH_KNOTS ( 'NONE', 3,
 ( #10235, #3786, #16929, #20209 ),
 .UNSPECIFIED., .F., .F.,
 ( 4, 4 ),
 ( 8.047005770514206345E-05, 0.0007531208497576732160 ),
 .UNSPECIFIED. ) ;
#17756 = DIRECTION ( 'NONE',  ( 0.000000000000000000, 0.000000000000000000, -1.000000000000000000 ) ) ;
#17757 = FACE_OUTER_BOUND ( 'NONE', #11703, .T. ) ;
#17758 = ORIENTED_EDGE ( 'NONE', *, *, #12280, .F. ) ;
#17759 = DIRECTION ( 'NONE',  ( -0.8660254037844380415, -0.5000000000000014433, -0.000000000000000000 ) ) ;
#17760 = FACE_OUTER_BOUND ( 'NONE', #8602, .T. ) ;
#17761 = DIRECTION ( 'NONE',  ( 0.000000000000000000, 0.000000000000000000, -1.000000000000000000 ) ) ;
#17762 = ORIENTED_EDGE ( 'NONE', *, *, #8314, .F. ) ;
#17763 = CARTESIAN_POINT ( 'NONE',  ( 200.2088966793999987, 0.2341713026616738524, -22.03054070023845767 ) ) ;
#17764 = CARTESIAN_POINT ( 'NONE',  ( 58.37797649651341203, 276.8427481158987007, -28.99999999999998934 ) ) ;
#17765 = CARTESIAN_POINT ( 'NONE',  ( 225.9078227465438147, 43.43157579942083402, -12.85003623376099213 ) ) ;
#17766 = AXIS2_PLACEMENT_3D ( 'NONE', #13840, #20286, #5751 ) ;
#17767 = CARTESIAN_POINT ( 'NONE',  ( 209.3990796341988982, 4.767305814873403769, -25.92587471718750436 ) ) ;
#17768 = EDGE_CURVE ( 'NONE', #19414, #15611, #7745, .T. ) ;
#17769 = CARTESIAN_POINT ( 'NONE',  ( -26.92128470956473407, 9.836181565225405876, -6.090021476509787313 ) ) ;
#17770 = ORIENTED_EDGE ( 'NONE', *, *, #6561, .T. ) ;
#17771 = CARTESIAN_POINT ( 'NONE',  ( 201.4752803508637271, 7.615505632025055149, -24.99940654434229970 ) ) ;
#17772 = PRESENTATION_STYLE_ASSIGNMENT (( #14718 ) ) ;
#17773 = CARTESIAN_POINT ( 'NONE',  ( -7.945426057903055117, 49.82671907149163815, -9.565339651835223833 ) ) ;
#17774 = CARTESIAN_POINT ( 'NONE',  ( 229.4945227733896331, 37.21922912141521778, -15.81459191843843293 ) ) ;
#17775 = CARTESIAN_POINT ( 'NONE',  ( 92.75906001725638816, 133.2929646387042339, 41.00000000000001421 ) ) ;
#17776 = EDGE_CURVE ( 'NONE', #3226, #13023, #15531, .T. ) ;
#17777 = CARTESIAN_POINT ( 'NONE',  ( -22.91475887178305015, 45.10727738977845291, -10.42048756752374672 ) ) ;
#17778 = VECTOR ( 'NONE', #5413, 1000.000000000000000 ) ;
#17780 = VERTEX_POINT ( 'NONE', #12644 ) ;
#17779 = ORIENTED_EDGE ( 'NONE', *, *, #9126, .T. ) ;
#17781 = VERTEX_POINT ( 'NONE', #19105 ) ;
#17782 = CARTESIAN_POINT ( 'NONE',  ( 30.10683012259193703, 5.000000000000000000, -4.999999999999997335 ) ) ;
#17783 = CARTESIAN_POINT ( 'NONE',  ( 202.3000072617431329, 22.83033358380322753, -2.044871543907030631 ) ) ;
#17784 = CARTESIAN_POINT ( 'NONE',  ( -6.621265648680998872, 79.74334935822896853, -9.599827418917257660 ) ) ;
#17785 = ORIENTED_EDGE ( 'NONE', *, *, #5886, .F. ) ;
#17786 = ORIENTED_EDGE ( 'NONE', *, *, #9487, .T. ) ;
#17787 = ORIENTED_EDGE ( 'NONE', *, *, #14435, .F. ) ;
#17788 = DIRECTION ( 'NONE',  ( -0.3654179821390598493, 0.6329225110641440999, -0.6825531432186625613 ) ) ;
#17789 = CARTESIAN_POINT ( 'NONE',  ( 214.4645575845060534, 14.93785843526373647, -7.327415643059550732 ) ) ;
#17790 = DIRECTION ( 'NONE',  ( -0.8660254037844358210, -0.5000000000000049960, 0.000000000000000000 ) ) ;
#17791 = CARTESIAN_POINT ( 'NONE',  ( 8.399999999999998579, 0.000000000000000000, 0.000000000000000000 ) ) ;
#17792 = VERTEX_POINT ( 'NONE', #5838 ) ;
#17793 = EDGE_CURVE ( 'NONE', #13143, #10497, #8839, .T. ) ;
#17794 = EDGE_LOOP ( 'NONE', ( #2854, #2312, #15348, #13081, #2217 ) ) ;
#17795 = EDGE_CURVE ( 'NONE', #10818, #6868, #9119, .T. ) ;
#17796 = DIRECTION ( 'NONE',  ( -0.000000000000000000, 1.000000000000000000, -0.000000000000000000 ) ) ;
#17797 = AXIS2_PLACEMENT_3D ( 'NONE', #2934, #4312, #4209 ) ;
#17798 = CONICAL_SURFACE ( 'NONE', #533, 4.999999999999995559, 1.029744258676653867 ) ;
#17799 = LINE ( 'NONE', #11854, #11480 ) ;
#17800 = CARTESIAN_POINT ( 'NONE',  ( 197.8063295462453652, -1.283151408128118565, -14.01039160325040989 ) ) ;
#17801 = CARTESIAN_POINT ( 'NONE',  ( -32.14365289034154927, 60.93336360728059731, 1.942657716202586426 ) ) ;
#17802 = CARTESIAN_POINT ( 'NONE',  ( 220.8209911524953384, 33.72570815222170637, -10.90641968010466911 ) ) ;
#17803 = ORIENTED_EDGE ( 'NONE', *, *, #17841, .T. ) ;
#17804 = CARTESIAN_POINT ( 'NONE',  ( 229.1599621875510024, 37.14574592179515378, -11.62239797051696577 ) ) ;
#17805 = DIRECTION ( 'NONE',  ( 0.8660254037844370423, 0.5000000000000026645, -0.000000000000000000 ) ) ;
#17806 = EDGE_LOOP ( 'NONE', ( #15226, #6511, #6153, #6908 ) ) ;
#17807 = AXIS2_PLACEMENT_3D ( 'NONE', #17141, #17455, #20619 ) ;
#17809 = EDGE_CURVE ( 'NONE', #17666, #18042, #4001, .T. ) ;
#17808 = CARTESIAN_POINT ( 'NONE',  ( 62.25477568219749003, 78.38020580725381592, -11.99461463175524756 ) ) ;
#17810 = ORIENTED_EDGE ( 'NONE', *, *, #10809, .F. ) ;
#17811 = AXIS2_PLACEMENT_3D ( 'NONE', #10144, #13677, #10255 ) ;
#17812 = LINE ( 'NONE', #3283, #14272 ) ;
#17813 = VECTOR ( 'NONE', #6543, 1000.000000000000000 ) ;
#17814 = CARTESIAN_POINT ( 'NONE',  ( 105.7973891242897650, 30.70991617951901986, -12.50000000000000000 ) ) ;
#17815 = EDGE_CURVE ( 'NONE', #10630, #14829, #14863, .T. ) ;
#17816 = DIRECTION ( 'NONE',  ( -0.5000000000000054401, 0.8660254037844354880, -0.000000000000000000 ) ) ;
#17817 = ORIENTED_EDGE ( 'NONE', *, *, #5912, .F. ) ;
#17818 = DIRECTION ( 'NONE',  ( -7.930164461608272272E-15, -3.965082230804136136E-15, -1.000000000000000000 ) ) ;
#17819 = ITEM_DEFINED_TRANSFORMATION ( 'NONE', 'NONE', #11122,  #18233 ) ;
#17820 = EDGE_CURVE ( 'NONE', #9718, #12634, #9432, .T. ) ;
#17821 = CARTESIAN_POINT ( 'NONE',  ( 59.39721438298058587, 215.0773763115390125, -22.00000000000000355 ) ) ;
#17822 = ORIENTED_EDGE ( 'NONE', *, *, #5637, .T. ) ;
#17823 = EDGE_CURVE ( 'NONE', #14739, #1146, #10759, .T. ) ;
#17824 = AXIS2_PLACEMENT_3D ( 'NONE', #3621, #11904, #13285 ) ;
#17825 = CARTESIAN_POINT ( 'NONE',  ( -31.82323003959540486, 64.25000000000000000, 2.481238266578627449 ) ) ;
#17826 = CARTESIAN_POINT ( 'NONE',  ( 211.4089789608015622, 27.46411792184940026, -14.32816039117628115 ) ) ;
#17827 = DIRECTION ( 'NONE',  ( 0.8660254037844360431, 0.5000000000000044409, -5.976026924694053325E-17 ) ) ;
#17828 = EDGE_CURVE ( 'NONE', #3383, #12912, #1402, .T. ) ;
#17829 = ADVANCED_FACE ( 'NONE', ( #9542 ), #4779, .F. ) ;
#17830 = AXIS2_PLACEMENT_3D ( 'NONE', #18626, #20206, #18204 ) ;
#17831 = CARTESIAN_POINT ( 'NONE',  ( 214.8858643771922630, 19.48210784701872811, -17.08769543353844611 ) ) ;
#17832 = CARTESIAN_POINT ( 'NONE',  ( 220.9052293801404403, 33.81574626886718704, -17.25078732088841349 ) ) ;
#17833 = VECTOR ( 'NONE', #18725, 1000.000000000000114 ) ;
#17834 = B_SPLINE_CURVE_WITH_KNOTS ( 'NONE', 3,
 ( #18373, #16568, #2050, #8502 ),
 .UNSPECIFIED., .F., .F.,
 ( 4, 4 ),
 ( 2.004673356297042134E-07, 0.0005365470222895969915 ),
 .UNSPECIFIED. ) ;
#17835 = DIRECTION ( 'NONE',  ( -0.8660254037844378194, -0.5000000000000013323, -0.000000000000000000 ) ) ;
#17836 = CARTESIAN_POINT ( 'NONE',  ( 4.000000000000000000, -1.759474945355379072, 3.047500000000001652 ) ) ;
#17837 = CARTESIAN_POINT ( 'NONE',  ( 221.8071444075225145, 32.25358361733145784, -12.96641767022729930 ) ) ;
#17838 = ORIENTED_EDGE ( 'NONE', *, *, #478, .F. ) ;
#17839 = ORIENTED_EDGE ( 'NONE', *, *, #536, .F. ) ;
#17841 = EDGE_CURVE ( 'NONE', #19523, #12371, #1634, .T. ) ;
#17840 = LINE ( 'NONE', #19721, #19972 ) ;
#17842 = CARTESIAN_POINT ( 'NONE',  ( 81.67385617171331091, 66.21413061234055419, 0.6300478184626461253 ) ) ;
#17843 = MANIFOLD_SOLID_BREP ( 'Fillet5', #9965 ) ;
#17844 = CARTESIAN_POINT ( 'NONE',  ( -13.69349610383069304, 70.93315970589998187, -4.447567583327517227 ) ) ;
#17845 = CARTESIAN_POINT ( 'NONE',  ( 75.16299901799432348, 52.17553498020845382, -14.69146284800536684 ) ) ;
#17847 = VERTEX_POINT ( 'NONE', #3049 ) ;
#17846 = ORIENTED_EDGE ( 'NONE', *, *, #1537, .T. ) ;
#17848 = VECTOR ( 'NONE', #13053, 1000.000000000000227 ) ;
#17849 =( NAMED_UNIT ( * ) SI_UNIT ( $, .STERADIAN. ) SOLID_ANGLE_UNIT ( ) );
#17850 = UNCERTAINTY_MEASURE_WITH_UNIT (LENGTH_MEASURE( 1.000000000000000082E-05 ), #19126, 'distance_accuracy_value', 'NONE');
#17851 = EDGE_CURVE ( 'NONE', #9495, #8582, #2276, .T. ) ;
#17852 = ORIENTED_EDGE ( 'NONE', *, *, #4060, .F. ) ;
#17853 = CARTESIAN_POINT ( 'NONE',  ( -32.98901474369844067, 73.25359183295174148, 0.03495786392106590285 ) ) ;
#17854 = EDGE_LOOP ( 'NONE', ( #19671, #14409, #13462, #9166 ) ) ;
#17855 = DIRECTION ( 'NONE',  ( 0.5000000000000057732, -0.8660254037844353769, 0.000000000000000000 ) ) ;
#17856 = CARTESIAN_POINT ( 'NONE',  ( -32.97826049705485474, 77.74400922168739214, -4.586390192070082250 ) ) ;
#17857 = LINE ( 'NONE', #16069, #20792 ) ;
#17858 = EDGE_CURVE ( 'NONE', #19247, #14393, #11257, .T. ) ;
#17859 = EDGE_LOOP ( 'NONE', ( #132, #20252 ) ) ;
#17860 = CARTESIAN_POINT ( 'NONE',  ( 222.1527769467159601, 32.06686066723883499, -13.49489896056993743 ) ) ;
#17861 = EDGE_CURVE ( 'NONE', #15334, #10335, #9085, .T. ) ;
#17862 = CARTESIAN_POINT ( 'NONE',  ( 77.94818390652243068, 67.33817290270525291, 0.2902393605762963458 ) ) ;
#17863 = AXIS2_PLACEMENT_3D ( 'NONE', #20231, #17072, #12188 ) ;
#17864 = FACE_OUTER_BOUND ( 'NONE', #4678, .T. ) ;
#17865 = ORIENTED_EDGE ( 'NONE', *, *, #968, .F. ) ;
#17866 =( REPRESENTATION_RELATIONSHIP ('NONE','NONE', #4634, #3951 ) REPRESENTATION_RELATIONSHIP_WITH_TRANSFORMATION ( #18994 )SHAPE_REPRESENTATION_RELATIONSHIP( ) );
#17867 = EDGE_CURVE ( 'NONE', #1053, #8779, #12297, .T. ) ;
#17869 = DIRECTION ( 'NONE',  ( 0.000000000000000000, 0.000000000000000000, -1.000000000000000000 ) ) ;
#17868 = VECTOR ( 'NONE', #13847, 1000.000000000000114 ) ;
#17870 = VERTEX_POINT ( 'NONE', #6215 ) ;
#17871 = CARTESIAN_POINT ( 'NONE',  ( 44.00000000000000000, -10.00000000000000000, 15.00000000000000000 ) ) ;
#17872 = ORIENTED_EDGE ( 'NONE', *, *, #295, .F. ) ;
#17873 = CARTESIAN_POINT ( 'NONE',  ( 209.1090394831926176, 31.29886781828238895, -12.47428928897383749 ) ) ;
#17874 = DIRECTION ( 'NONE',  ( 0.000000000000000000, 0.000000000000000000, -1.000000000000000000 ) ) ;
#17875 = CARTESIAN_POINT ( 'NONE',  ( 208.8107687779840944, 4.427644383670621409, -14.00000000000005507 ) ) ;
#17876 = EDGE_CURVE ( 'NONE', #16527, #631, #19248, .T. ) ;
#17877 = LINE ( 'NONE', #11500, #4929 ) ;
#17878 = AXIS2_PLACEMENT_3D ( 'NONE', #9792, #1758, #16185 ) ;
#17879 = CARTESIAN_POINT ( 'NONE',  ( 208.1960812450810465, 4.072754371081502178, -2.075899210536066963 ) ) ;
#17880 = DIRECTION ( 'NONE',  ( 0.8660254037844375974, 0.5000000000000019984, -2.775557561562891844E-16 ) ) ;
#17881 = VERTEX_POINT ( 'NONE', #1259 ) ;
#17882 = VECTOR ( 'NONE', #19847, 1000.000000000000114 ) ;
#17883 = CARTESIAN_POINT ( 'NONE',  ( 65.28213910571976442, 76.58029512791007676, -19.23060072459815828 ) ) ;
#17884 = CARTESIAN_POINT ( 'NONE',  ( -4.179710852470351234, 56.67225486372360876, 4.072319667107016983 ) ) ;
#17885 = ORIENTED_EDGE ( 'NONE', *, *, #8711, .T. ) ;
#17886 = CARTESIAN_POINT ( 'NONE',  ( 209.7235900860870572, 27.11634112578974154, -16.89203719259520753 ) ) ;
#17887 = CARTESIAN_POINT ( 'NONE',  ( -8.109701803253319241, 50.18354407797716732, -14.84573819736936784 ) ) ;
#17888 = CARTESIAN_POINT ( 'NONE',  ( -11.36219877386465882, 79.99567133403120067, -12.08300025664926558 ) ) ;
#17889 = LINE ( 'NONE', #14925, #19609 ) ;
#17890 = CARTESIAN_POINT ( 'NONE',  ( 29.50490953756714063, 242.8523670591319785, -8.999999999999953815 ) ) ;
#17891 = B_SPLINE_CURVE_WITH_KNOTS ( 'NONE', 3,
 ( #2417, #13980, #5787, #2313 ),
 .UNSPECIFIED., .F., .F.,
 ( 4, 4 ),
 ( 4.655683356685539183E-05, 0.0006124830558495551617 ),
 .UNSPECIFIED. ) ;
#17892 = AXIS2_PLACEMENT_3D ( 'NONE', #8922, #15418, #872 ) ;
#17893 = EDGE_CURVE ( 'NONE', #12774, #10573, #14312, .T. ) ;
#17894 = VECTOR ( 'NONE', #15603, 1000.000000000000114 ) ;
#17896 = ORIENTED_EDGE ( 'NONE', *, *, #9660, .T. ) ;
#17895 = EDGE_LOOP ( 'NONE', ( #5804, #13777, #18922, #13617 ) ) ;
#17897 = ORIENTED_EDGE ( 'NONE', *, *, #1526, .F. ) ;
#17898 = CARTESIAN_POINT ( 'NONE',  ( -78.28193223680408153, 135.5882839488078844, -1.028642961561239307E-12 ) ) ;
#17899 = DIRECTION ( 'NONE',  ( 0.8660254037844355990, 0.5000000000000054401, 0.000000000000000000 ) ) ;
#17900 = ORIENTED_EDGE ( 'NONE', *, *, #20653, .T. ) ;
#17901 = DIRECTION ( 'NONE',  ( 0.8660254037844352659, 0.5000000000000056621, 0.000000000000000000 ) ) ;
#17902 = DIRECTION ( 'NONE',  ( -0.4711304610594141407, 0.8160218955482504422, 0.3348796121709771700 ) ) ;
#17903 = CARTESIAN_POINT ( 'NONE',  ( 59.39721438298058587, 215.0773763115390125, -22.00000000000000355 ) ) ;
#17904 = FACE_OUTER_BOUND ( 'NONE', #1915, .T. ) ;
#17905 = VERTEX_POINT ( 'NONE', #1049 ) ;
#17906 = ORIENTED_EDGE ( 'NONE', *, *, #17248, .T. ) ;
#17907 = CARTESIAN_POINT ( 'NONE',  ( 199.3859296228393134, 5.878169164976177363, -24.01557619556968248 ) ) ;
#17908 = EDGE_CURVE ( 'NONE', #5642, #8941, #4641, .T. ) ;
#17909 = AXIS2_PLACEMENT_3D ( 'NONE', #12348, #18801, #12237 ) ;
#17910 = DIRECTION ( 'NONE',  ( 0.5000000000000029976, -0.8660254037844370423, 0.000000000000000000 ) ) ;
#17911 = CARTESIAN_POINT ( 'NONE',  ( 204.4254563108872844, 13.44278843410413771, -2.187257959407755248 ) ) ;
#17912 = CARTESIAN_POINT ( 'NONE',  ( -27.32435382328680262, 62.88336031010526028, 5.293632132712875915 ) ) ;
#17913 = FACE_OUTER_BOUND ( 'NONE', #7720, .T. ) ;
#17914 = ADVANCED_FACE ( 'NONE', ( #20330 ), #5417, .F. ) ;
#17915 = FACE_OUTER_BOUND ( 'NONE', #17381, .T. ) ;
#17916 = CARTESIAN_POINT ( 'NONE',  ( 208.5220424616560422, 2.921106821514924512, -14.00000000000005507 ) ) ;
#17917 = ADVANCED_FACE ( 'NONE', ( #5638 ), #5538, .T. ) ;
#17918 = ORIENTED_EDGE ( 'NONE', *, *, #5992, .F. ) ;
#17919 = CARTESIAN_POINT ( 'NONE',  ( 65.40372546169420787, 76.50785360310598548, -5.659300543005241657 ) ) ;
#17920 = ADVANCED_FACE ( 'NONE', ( #10409, #4174 ), #13721, .F. ) ;
#17921 = ORIENTED_EDGE ( 'NONE', *, *, #13036, .F. ) ;
#17922 = CIRCLE ( 'NONE', #3674, 3.619616396367202782 ) ;
#17923 = CARTESIAN_POINT ( 'NONE',  ( -0.1835594872087454865, 65.48968590022838043, 2.492004793192846179 ) ) ;
#17924 = CARTESIAN_POINT ( 'NONE',  ( 217.3449329263786467, 38.26293602756121004, -15.69686519029799676 ) ) ;
#17925 = ORIENTED_EDGE ( 'NONE', *, *, #856, .T. ) ;
#17926 = DIRECTION ( 'NONE',  ( 0.5000000000000034417, -0.8660254037844364872, 0.000000000000000000 ) ) ;
#17927 = DIRECTION ( 'NONE',  ( -0.5000000000000047740, 0.8660254037844358210, 0.000000000000000000 ) ) ;
#17928 = EDGE_LOOP ( 'NONE', ( #15967, #3082, #239, #11161 ) ) ;
#17929 = FACE_OUTER_BOUND ( 'NONE', #6634, .T. ) ;
#17930 = CARTESIAN_POINT ( 'NONE',  ( 195.2585560139913810, 8.150276080056761074, -20.52105855319921446 ) ) ;
#17931 = AXIS2_PLACEMENT_3D ( 'NONE', #19256, #6402, #4527 ) ;
#17932 = ORIENTED_EDGE ( 'NONE', *, *, #2209, .F. ) ;
#17933 = CARTESIAN_POINT ( 'NONE',  ( 58.65319233816361333, 85.44060140440096518, -13.53501203742773029 ) ) ;
#17934 = FACE_OUTER_BOUND ( 'NONE', #1877, .T. ) ;
#17935 = B_SPLINE_CURVE_WITH_KNOTS ( 'NONE', 3,
 ( #20137, #7516, #4137, #5598, #8997, #851, #12087, #4023, #14007, #16966, #13788, #5702, #12194, #20450, #5916, #18871, #17704, #9410 ),
 .UNSPECIFIED., .F., .F.,
 ( 4, 2, 2, 2, 2, 2, 2, 2, 4 ),
 ( 0.02369296886942158509, 0.02467920192125608314, 0.02566543497309058119, 0.02665166802492507578, 0.02763790107675957383, 0.02862413412859407189, 0.02961036718042856647, 0.03059660023226306452, 0.03158283328409756258 ),
 .UNSPECIFIED. ) ;
#17936 = ADVANCED_FACE ( 'NONE', ( #8833 ), #7551, .F. ) ;
#17937 = DIRECTION ( 'NONE',  ( 0.8426815769442684845, 0.4865224352899188420, 0.2306158707424263155 ) ) ;
#17938 = FACE_OUTER_BOUND ( 'NONE', #9887, .T. ) ;
#17939 = CARTESIAN_POINT ( 'NONE',  ( 221.6641179803099249, 32.29539445528372710, -12.98880265512673304 ) ) ;
#17940 = EDGE_CURVE ( 'NONE', #16469, #1522, #14534, .T. ) ;
#17941 = VERTEX_POINT ( 'NONE', #2486 ) ;
#17942 = CARTESIAN_POINT ( 'NONE',  ( 208.0983737146324870, 5.661548828456886895, -14.00000000000005507 ) ) ;
#17943 = CIRCLE ( 'NONE', #2036, 5.400000000000040323 ) ;
#17944 = CARTESIAN_POINT ( 'NONE',  ( 61.96862002106807665, 82.88931969431537539, -6.034168607505590032 ) ) ;
#17945 = DIRECTION ( 'NONE',  ( -0.8660254037844370423, -0.5000000000000026645, 0.000000000000000000 ) ) ;
#17946 = CARTESIAN_POINT ( 'NONE',  ( 75.56440020197395313, 52.70843083039871857, -8.259164681586764090 ) ) ;
#17948 = VERTEX_POINT ( 'NONE', #17005 ) ;
#17947 = ORIENTED_EDGE ( 'NONE', *, *, #1409, .T. ) ;
#17949 = EDGE_CURVE ( 'NONE', #9470, #14657, #10299, .T. ) ;
#17950 = ORIENTED_EDGE ( 'NONE', *, *, #18302, .T. ) ;
#17951 = ORIENTED_EDGE ( 'NONE', *, *, #20857, .F. ) ;
#17952 = AXIS2_PLACEMENT_3D ( 'NONE', #13217, #4937, #17681 ) ;
#17953 = CARTESIAN_POINT ( 'NONE',  ( -15.99999999999999289, -10.00000000000000000, 0.000000000000000000 ) ) ;
#17954 = VERTEX_POINT ( 'NONE', #20484 ) ;
#17955 = CARTESIAN_POINT ( 'NONE',  ( 198.4028805101389992, 5.310605495132000975, -23.06309126349794170 ) ) ;
#17956 = EDGE_CURVE ( 'NONE', #8753, #15844, #16893, .T. ) ;
#17957 = CARTESIAN_POINT ( 'NONE',  ( 188.9132435853528591, 28.89116896218935082, -14.00000000000004086 ) ) ;
#17958 = EDGE_CURVE ( 'NONE', #3255, #14554, #13829, .T. ) ;
#17959 = CARTESIAN_POINT ( 'NONE',  ( 80.91283318083826259, 65.19299774870088982, 0.5000000000000999201 ) ) ;
#17960 = CARTESIAN_POINT ( 'NONE',  ( 208.5178070548358278, 11.68151032033851600, -25.34310559273333396 ) ) ;
#17961 = EDGE_LOOP ( 'NONE', ( #10532, #14888, #11685, #19695 ) ) ;
#17962 = CIRCLE ( 'NONE', #17282, 5.000000000000039968 ) ;
#17963 = DIRECTION ( 'NONE',  ( -0.8660254037844378194, -0.5000000000000013323, -0.000000000000000000 ) ) ;
#17964 = DIRECTION ( 'NONE',  ( 0.8660254037844355990, 0.5000000000000054401, 0.000000000000000000 ) ) ;
#17965 = CONICAL_SURFACE ( 'NONE', #19975, 13.07248899748297433, 0.6693469023067423196 ) ;
#17966 = VERTEX_POINT ( 'NONE', #5851 ) ;
#17967 = CARTESIAN_POINT ( 'NONE',  ( 227.6096221818959009, 40.48397271309900702, -10.44704522969157345 ) ) ;
#17968 = AXIS2_PLACEMENT_3D ( 'NONE', #8888, #739, #16743 ) ;
#17969 = EDGE_CURVE ( 'NONE', #4227, #19623, #15539, .T. ) ;
#17970 = VERTEX_POINT ( 'NONE', #4059 ) ;
#17971 = ADVANCED_FACE ( 'NONE', ( #3853 ), #7239, .F. ) ;
#17972 = CARTESIAN_POINT ( 'NONE',  ( 209.6243204174557206, 3.018531609524862880, -14.00000000000005507 ) ) ;
#17973 = DIRECTION ( 'NONE',  ( -0.000000000000000000, -1.000000000000000000, -0.000000000000000000 ) ) ;
#17974 = CARTESIAN_POINT ( 'NONE',  ( 218.8765682739957583, 37.74142054458803131, -16.83383072344315678 ) ) ;
#17975 = VECTOR ( 'NONE', #1014, 1000.000000000000114 ) ;
#17976 = VECTOR ( 'NONE', #11743, 999.9999999999998863 ) ;
#17977 = DIRECTION ( 'NONE',  ( -0.8660254037844360431, -0.5000000000000045519, -4.336808689942050277E-16 ) ) ;
#17978 = DIRECTION ( 'NONE',  ( 0.1992005449231252778, -0.3450254647022570897, -0.9172113015054499385 ) ) ;
#17979 = AXIS2_PLACEMENT_3D ( 'NONE', #11520, #8112, #3357 ) ;
#17980 = CARTESIAN_POINT ( 'NONE',  ( -43.39423452328062325, 75.16101894988052834, 104.1461628558723760 ) ) ;
#17981 = EDGE_CURVE ( 'NONE', #20478, #18457, #996, .T. ) ;
#17982 = VERTEX_POINT ( 'NONE', #7440 ) ;
#17983 = VECTOR ( 'NONE', #19268, 1000.000000000000114 ) ;
#17984 = CARTESIAN_POINT ( 'NONE',  ( 78.92217576635638920, 67.90907104038892328, -25.20063723745943207 ) ) ;
#17985 = CARTESIAN_POINT ( 'NONE',  ( -4.485171960567237548, 45.77964704178626221, -4.920232212067642941 ) ) ;
#17986 = ORIENTED_EDGE ( 'NONE', *, *, #9145, .T. ) ;
#17987 = CARTESIAN_POINT ( 'NONE',  ( 207.7157532681331134, 10.68739508888871548, -1.717498466822861225 ) ) ;
#17988 = CARTESIAN_POINT ( 'NONE',  ( 0.3192688095861958009, 59.91499571937752933, 1.616389984123141721 ) ) ;
#17989 = LINE ( 'NONE', #9904, #15385 ) ;
#17990 = EDGE_CURVE ( 'NONE', #8848, #5086, #11134, .T. ) ;
#17991 = CARTESIAN_POINT ( 'NONE',  ( 195.6523656023913702, 4.253644234526245071, -11.09368851308730974 ) ) ;
#17992 = AXIS2_PLACEMENT_3D ( 'NONE', #5778, #14186, #12479 ) ;
#17993 = DIRECTION ( 'NONE',  ( 0.5000000000000055511, -0.8660254037844353769, 1.110223024625156417E-16 ) ) ;
#17995 = ORIENTED_EDGE ( 'NONE', *, *, #8998, .F. ) ;
#17994 = ORIENTED_EDGE ( 'NONE', *, *, #13502, .F. ) ;
#17996 = ORIENTED_EDGE ( 'NONE', *, *, #6271, .F. ) ;
#17997 = DIRECTION ( 'NONE',  ( 0.000000000000000000, -0.5000000000000018874, -0.8660254037844374864 ) ) ;
#17999 = CARTESIAN_POINT ( 'NONE',  ( 169.8972143829816730, 23.68576207517868326, -14.00000000000007461 ) ) ;
#17998 = CIRCLE ( 'NONE', #12252, 12.47473710546057823 ) ;
#18000 = EDGE_LOOP ( 'NONE', ( #11387, #2099, #6850, #16207 ) ) ;
#18001 = ORIENTED_EDGE ( 'NONE', *, *, #20424, .T. ) ;
#18002 = LINE ( 'NONE', #3470, #3441 ) ;
#18003 = CARTESIAN_POINT ( 'NONE',  ( 28.51452848080068847, 214.5677573683055357, -14.00000000000002842 ) ) ;
#18004 = CARTESIAN_POINT ( 'NONE',  ( 218.5174457518189968, 38.15746093317041954, -12.00039960601313282 ) ) ;
#18005 = LINE ( 'NONE', #6528, #16457 ) ;
#18006 = ORIENTED_EDGE ( 'NONE', *, *, #4339, .F. ) ;
#18007 = ORIENTED_EDGE ( 'NONE', *, *, #591, .T. ) ;
#18008 = CARTESIAN_POINT ( 'NONE',  ( 200.4364383576235866, 6.484680665789935183, -3.188775577416750995 ) ) ;
#18009 = DIRECTION ( 'NONE',  ( -0.8528685319524407227, -0.4924038765061096168, -0.1736481776669271115 ) ) ;
#18010 = VECTOR ( 'NONE', #9811, 1000.000000000000000 ) ;
#18011 = VECTOR ( 'NONE', #4245, 1000.000000000000000 ) ;
#18012 = CARTESIAN_POINT ( 'NONE',  ( 84.99529059433410794, 176.7402077374548526, 11.00000000000001066 ) ) ;
#18013 = CARTESIAN_POINT ( 'NONE',  ( -28.31427895950539408, 52.41482254867882062, 2.195225357249351639 ) ) ;
#18014 = LINE ( 'NONE', #13453, #14337 ) ;
#18015 = ORIENTED_EDGE ( 'NONE', *, *, #4432, .T. ) ;
#18016 = PLANE ( 'NONE',  #7453 ) ;
#18017 = DIRECTION ( 'NONE',  ( 0.5000000000000038858, -0.8660254037844362651, 0.000000000000000000 ) ) ;
#18018 = ORIENTED_EDGE ( 'NONE', *, *, #11119, .F. ) ;
#18019 = CARTESIAN_POINT ( 'NONE',  ( 62.64650668844161885, 78.15169325881764451, -12.59136457139523380 ) ) ;
#18020 = EDGE_LOOP ( 'NONE', ( #11841, #18018, #10038, #12082, #8068, #14574, #19726, #7881 ) ) ;
#18021 = VERTEX_POINT ( 'NONE', #4280 ) ;
#18022 = CARTESIAN_POINT ( 'NONE',  ( 208.1960812450810465, 4.072754371081502178, -2.075899210536066963 ) ) ;
#18023 = DIRECTION ( 'NONE',  ( 0.8660254037844370423, 0.5000000000000026645, -0.000000000000000000 ) ) ;
#18024 = CIRCLE ( 'NONE', #4133, 12.47473710546057823 ) ;
#18025 = AXIS2_PLACEMENT_3D ( 'NONE', #11752, #826, #7073 ) ;
#18026 = ORIENTED_EDGE ( 'NONE', *, *, #10228, .T. ) ;
#18027 = PLANE ( 'NONE',  #20537 ) ;
#18028 = CARTESIAN_POINT ( 'NONE',  ( -31.34819206192207020, 65.74999999999998579, 2.481238266578628338 ) ) ;
#18029 = EDGE_LOOP ( 'NONE', ( #8172, #2399, #13647 ) ) ;
#18030 = EDGE_CURVE ( 'NONE', #6684, #16010, #9136, .T. ) ;
#18031 = CARTESIAN_POINT ( 'NONE',  ( 204.1847125716027733, 2.529609678273321727, -2.551678190571418092 ) ) ;
#18032 = CARTESIAN_POINT ( 'NONE',  ( 26.99999999999999645, 65.00000000000000000, -12.50000000000000000 ) ) ;
#18033 = VERTEX_POINT ( 'NONE', #9240 ) ;
#18034 = DIRECTION ( 'NONE',  ( -0.1348983855785130803, 0.2336508576809998017, 0.9629172873477991335 ) ) ;
#18035 = LINE ( 'NONE', #8476, #2458 ) ;
#18036 = AXIS2_PLACEMENT_3D ( 'NONE', #15505, #15402, #14011 ) ;
#18037 = VERTEX_POINT ( 'NONE', #17529 ) ;
#18038 = CARTESIAN_POINT ( 'NONE',  ( 208.5367637565365158, 11.69245497716835480, -16.77975104236438497 ) ) ;
#18039 = AXIS2_PLACEMENT_3D ( 'NONE', #8657, #8551, #10556 ) ;
#18040 = CARTESIAN_POINT ( 'NONE',  ( 225.7841225803420855, 42.99287163968411818, -13.51412976915880826 ) ) ;
#18041 = CARTESIAN_POINT ( 'NONE',  ( 205.8264633344831225, 9.596613037118636669, -14.00000000000005507 ) ) ;
#18042 = VERTEX_POINT ( 'NONE', #14470 ) ;
#18043 = AXIS2_PLACEMENT_3D ( 'NONE', #5683, #8880, #5370 ) ;
#18044 = CARTESIAN_POINT ( 'NONE',  ( 177.1791022559528983, 56.75747545832872731, 0.9999999999999431566 ) ) ;
#18045 = CARTESIAN_POINT ( 'NONE',  ( 190.7433706042750146, 35.72129598111152404, -9.000000000000062172 ) ) ;
#18046 = EDGE_CURVE ( 'NONE', #1440, #1135, #7597, .T. ) ;
#18047 = CARTESIAN_POINT ( 'NONE',  ( 221.4896362261276863, 32.59760571852110189, -15.81459191843843648 ) ) ;
#18048 = CARTESIAN_POINT ( 'NONE',  ( 75.43643680125984474, 52.53826089850589653, -16.21113233865809988 ) ) ;
#18049 = ORIENTED_EDGE ( 'NONE', *, *, #3706, .F. ) ;
#18050 = ORIENTED_EDGE ( 'NONE', *, *, #16921, .F. ) ;
#18051 = ORIENTED_EDGE ( 'NONE', *, *, #3566, .T. ) ;
#18052 = CIRCLE ( 'NONE', #16363, 3.902363844300875240 ) ;
#18053 = EDGE_CURVE ( 'NONE', #17781, #18441, #9447, .T. ) ;
#18054 = PLANE ( 'NONE',  #17824 ) ;
#18055 = ORIENTED_EDGE ( 'NONE', *, *, #17348, .T. ) ;
#18056 = CARTESIAN_POINT ( 'NONE',  ( 227.9603656397142402, 39.54999814776896017, -10.29768792660755139 ) ) ;
#18057 = EDGE_CURVE ( 'NONE', #6684, #6371, #7738, .T. ) ;
#18058 = CARTESIAN_POINT ( 'NONE',  ( -15.99999999999999289, 79.99999999999998579, -12.50000000000000000 ) ) ;
#18059 = CARTESIAN_POINT ( 'NONE',  ( 219.3753053876406511, 36.25973415479045059, -17.38313153181858084 ) ) ;
#18060 = DIRECTION ( 'NONE',  ( 0.5000000000000052180, -0.8660254037844355990, 2.220446049250312341E-16 ) ) ;
#18061 = CARTESIAN_POINT ( 'NONE',  ( 218.2759540644739502, 38.13384169582290895, -15.28456752314048828 ) ) ;
#18062 = EDGE_CURVE ( 'NONE', #8661, #5484, #1322, .T. ) ;
#18063 = DIRECTION ( 'NONE',  ( -0.8660254037844354880, -0.5000000000000055511, 0.000000000000000000 ) ) ;
#18064 = PLANE ( 'NONE',  #19223 ) ;
#18065 = VERTEX_POINT ( 'NONE', #6369 ) ;
#18066 = AXIS2_PLACEMENT_3D ( 'NONE', #4777, #9642, #1500 ) ;
#18067 = AXIS2_PLACEMENT_3D ( 'NONE', #15831, #15633, #5844 ) ;
#18068 = CARTESIAN_POINT ( 'NONE',  ( 30.00000000000000000, 0.000000000000000000, 28.99999999999999645 ) ) ;
#18069 = PLANE ( 'NONE',  #13566 ) ;
#18070 = DIRECTION ( 'NONE',  ( -0.5566703992264088185, -0.3213938048432679051, 0.7660444431189864511 ) ) ;
#18071 = ADVANCED_FACE ( 'NONE', ( #9560 ), #2333, .F. ) ;
#18072 = ORIENTED_EDGE ( 'NONE', *, *, #536, .T. ) ;
#18073 = CARTESIAN_POINT ( 'NONE',  ( 209.0398851729401315, 31.46936297222353929, -12.74687664482581795 ) ) ;
#18074 = LINE ( 'NONE', #2274, #10187 ) ;
#18075 = CARTESIAN_POINT ( 'NONE',  ( 205.8311783259423464, 2.707377034109388347, -2.561001429077326197 ) ) ;
#18076 = ADVANCED_FACE ( 'NONE', ( #3113 ), #7659, .T. ) ;
#18077 = DIRECTION ( 'NONE',  ( -0.8640469734401363677, -0.5034111914617517280, 1.224637277265100606E-16 ) ) ;
#18078 = CARTESIAN_POINT ( 'NONE',  ( -27.75418142457269255, 9.358687574860853786, -4.265973664729101777 ) ) ;
#18079 = DIRECTION ( 'NONE',  ( 0.1674398060854888903, -0.2900142513495467256, 0.9422609221188237294 ) ) ;
#18080 = ORIENTED_EDGE ( 'NONE', *, *, #17809, .F. ) ;
#18081 = CARTESIAN_POINT ( 'NONE',  ( 66.12090498588680987, 76.08041367800895216, -19.94911872569857891 ) ) ;
#18082 = CARTESIAN_POINT ( 'NONE',  ( -10.76567231371678268, 45.28977633731097541, -11.35779591101546870 ) ) ;
#18083 = ADVANCED_FACE ( 'NONE', ( #2902 ), #12864, .T. ) ;
#18084 = EDGE_CURVE ( 'NONE', #4912, #3287, #13167, .T. ) ;
#18085 = ADVANCED_FACE ( 'NONE', ( #7761 ), #19020, .F. ) ;
#18086 = ORIENTED_EDGE ( 'NONE', *, *, #8425, .T. ) ;
#18087 = DIRECTION ( 'NONE',  ( 0.8660254037844369313, 0.5000000000000027756, 0.000000000000000000 ) ) ;
#18088 = CARTESIAN_POINT ( 'NONE',  ( 1.421481300724954044, 54.47125872025552695, -1.791815321364545799 ) ) ;
#18089 = CARTESIAN_POINT ( 'NONE',  ( 226.2284856962982360, 42.87617127834123210, -14.91677899116113082 ) ) ;
#18090 = LINE ( 'NONE', #2085, #19332 ) ;
#18091 = CARTESIAN_POINT ( 'NONE',  ( 229.7731284206632836, 36.73666998506165982, -16.20791459969597881 ) ) ;
#18092 = DIRECTION ( 'NONE',  ( 0.000000000000000000, -6.938893903907177533E-18, -1.000000000000000000 ) ) ;
#18094 = ORIENTED_EDGE ( 'NONE', *, *, #13801, .F. ) ;
#18093 = ORIENTED_EDGE ( 'NONE', *, *, #20526, .F. ) ;
#18095 = ORIENTED_EDGE ( 'NONE', *, *, #1283, .F. ) ;
#18096 = VERTEX_POINT ( 'NONE', #17744 ) ;
#18097 = AXIS2_PLACEMENT_3D ( 'NONE', #586, #19862, #18281 ) ;
#18098 = DIRECTION ( 'NONE',  ( 0.5000000000000007772, -0.8660254037844381525, 0.000000000000000000 ) ) ;
#18099 = DIRECTION ( 'NONE',  ( 0.5000000000000054401, -0.8660254037844354880, 0.000000000000000000 ) ) ;
#18100 = EDGE_CURVE ( 'NONE', #15951, #10374, #3207, .T. ) ;
#18101 = ORIENTED_EDGE ( 'NONE', *, *, #9247, .T. ) ;
#18102 = ORIENTED_EDGE ( 'NONE', *, *, #583, .T. ) ;
#18103 = CARTESIAN_POINT ( 'NONE',  ( -19.99317890361201577, 61.82300078473741678, -3.011576861204080746 ) ) ;
#18104 = CARTESIAN_POINT ( 'NONE',  ( 229.4255421505970958, 36.68574793232696862, -12.51312656967083115 ) ) ;
#18105 = CARTESIAN_POINT ( 'NONE',  ( -11.72929844504693442, 63.53565811406050301, -2.601344003386943715 ) ) ;
#18106 = ORIENTED_EDGE ( 'NONE', *, *, #6141, .F. ) ;
#18107 = ORIENTED_EDGE ( 'NONE', *, *, #11302, .T. ) ;
#18108 = FACE_OUTER_BOUND ( 'NONE', #2783, .T. ) ;
#18109 = ADVANCED_FACE ( 'NONE', ( #9664 ), #15496, .F. ) ;
#18110 = CARTESIAN_POINT ( 'NONE',  ( -31.74999999999995737, 5.776289300541449237E-16, -5.000000000000036415 ) ) ;
#18111 = EDGE_CURVE ( 'NONE', #18707, #13470, #9074, .T. ) ;
#18112 = ADVANCED_FACE ( 'NONE', ( #3524 ), #13390, .T. ) ;
#18113 = DIRECTION ( 'NONE',  ( -0.8660254037844361541, -0.5000000000000042188, -3.026831728535680894E-16 ) ) ;
#18114 = CARTESIAN_POINT ( 'NONE',  ( -33.02519701587559098, 51.39208029789107002, -6.179649924386284354 ) ) ;
#18115 = CARTESIAN_POINT ( 'NONE',  ( 228.1017308963826622, 39.63161541676052479, -10.43865930680574827 ) ) ;
#18116 = EDGE_LOOP ( 'NONE', ( #758, #1255, #14545, #18933 ) ) ;
#18117 = DIRECTION ( 'NONE',  ( 1.000000000000000000, 0.000000000000000000, -0.000000000000000000 ) ) ;
#18118 = CARTESIAN_POINT ( 'NONE',  ( 33.39482959517242477, 266.1148278819781581, 4.841106397986906451 ) ) ;
#18119 = ORIENTED_EDGE ( 'NONE', *, *, #15159, .F. ) ;
#18120 = CARTESIAN_POINT ( 'NONE',  ( 60.51398719102741097, 84.00985113818899208, -7.546147954418239046 ) ) ;
#18121 = EDGE_LOOP ( 'NONE', ( #18150, #12447, #8109, #2467, #19062, #2855 ) ) ;
#18122 = CARTESIAN_POINT ( 'NONE',  ( 198.3196067457501783, -0.8566107491083605474, -18.25196083293855409 ) ) ;
#18123 = DIRECTION ( 'NONE',  ( 0.000000000000000000, 0.9123518090004750780, -0.4094071037653847500 ) ) ;
#18124 = AXIS2_PLACEMENT_3D ( 'NONE', #2471, #8924, #15420 ) ;
#18125 = ORIENTED_EDGE ( 'NONE', *, *, #16894, .F. ) ;
#18126 = CARTESIAN_POINT ( 'NONE',  ( 220.0479314030272064, 35.09471172164835906, -17.56803216753791475 ) ) ;
#18127 = ORIENTED_EDGE ( 'NONE', *, *, #17043, .T. ) ;
#18128 = AXIS2_PLACEMENT_3D ( 'NONE', #16754, #5602, #7205 ) ;
#18129 = CARTESIAN_POINT ( 'NONE',  ( -29.98061410047647257, 65.74999999999995737, 2.827122728375906835 ) ) ;
#18130 = ORIENTED_EDGE ( 'NONE', *, *, #8178, .T. ) ;
#18131 = CARTESIAN_POINT ( 'NONE',  ( 4.000000000000000000, 5.278424836066145431, -3.047500000000006093 ) ) ;
#18132 = DIRECTION ( 'NONE',  ( -0.8660254037844361541, -0.5000000000000044409, 0.000000000000000000 ) ) ;
#18133 = DIRECTION ( 'NONE',  ( 0.5000000000000049960, -0.8660254037844358210, 0.000000000000000000 ) ) ;
#18134 = DIRECTION ( 'NONE',  ( 0.5000000000000054401, -0.8660254037844354880, 0.000000000000000000 ) ) ;
#18135 = ORIENTED_EDGE ( 'NONE', *, *, #9858, .F. ) ;
#18136 = CARTESIAN_POINT ( 'NONE',  ( 30.00000000000000000, 5.000000000000000000, 30.00000000000000000 ) ) ;
#18137 = PLANE ( 'NONE',  #12676 ) ;
#18138 = DIRECTION ( 'NONE',  ( -0.5000000000000054401, 0.8660254037844354880, -0.000000000000000000 ) ) ;
#18139 = AXIS2_PLACEMENT_3D ( 'NONE', #17268, #20754, #6323 ) ;
#18140 = ORIENTED_EDGE ( 'NONE', *, *, #4597, .F. ) ;
#18141 = VECTOR ( 'NONE', #7834, 1000.000000000000114 ) ;
#18142 = CARTESIAN_POINT ( 'NONE',  ( 205.5965122587965084, 9.994899983462953941, -14.00000000000005507 ) ) ;
#18143 = CARTESIAN_POINT ( 'NONE',  ( 202.9102931164051711, 24.36002564953663097, -12.80119896869108764 ) ) ;
#18144 = B_SPLINE_CURVE_WITH_KNOTS ( 'NONE', 3,
 ( #17771, #16189, #20735, #8097 ),
 .UNSPECIFIED., .F., .F.,
 ( 4, 4 ),
 ( 3.628021920466675907E-05, 0.0007089310112617852253 ),
 .UNSPECIFIED. ) ;
#18145 = EDGE_CURVE ( 'NONE', #13448, #6800, #18260, .T. ) ;
#18146 = ORIENTED_EDGE ( 'NONE', *, *, #16424, .T. ) ;
#18147 = FACE_OUTER_BOUND ( 'NONE', #4403, .T. ) ;
#18148 = CARTESIAN_POINT ( 'NONE',  ( 75.02715018211347342, 51.99577528146775762, -12.09344144936138399 ) ) ;
#18150 = ORIENTED_EDGE ( 'NONE', *, *, #10953, .F. ) ;
#18149 = ORIENTED_EDGE ( 'NONE', *, *, #16978, .T. ) ;
#18151 = VERTEX_POINT ( 'NONE', #8607 ) ;
#18152 = CIRCLE ( 'NONE', #9002, 9.999999999999998224 ) ;
#18153 = ORIENTED_EDGE ( 'NONE', *, *, #13219, .T. ) ;
#18154 = CARTESIAN_POINT ( 'NONE',  ( 5.000000000000000000, 4.969004387540385421E-16, -4.057500000000000107 ) ) ;
#18155 = ORIENTED_EDGE ( 'NONE', *, *, #6658, .F. ) ;
#18156 = AXIS2_PLACEMENT_3D ( 'NONE', #17379, #11013, #2859 ) ;
#18157 = CARTESIAN_POINT ( 'NONE',  ( 77.43461555835260413, 55.23580102254843638, -3.894515596738437946 ) ) ;
#18158 = CIRCLE ( 'NONE', #18830, 12.47473710546057823 ) ;
#18159 = CARTESIAN_POINT ( 'NONE',  ( -20.05080448500343238, 80.00000000000873968, -11.83620004860030939 ) ) ;
#18160 = FACE_OUTER_BOUND ( 'NONE', #18592, .T. ) ;
#18161 = CARTESIAN_POINT ( 'NONE',  ( 218.5440333250598997, 38.31738797143729869, -16.00491213559310921 ) ) ;
#18162 = VERTEX_POINT ( 'NONE', #8712 ) ;
#18163 = ADVANCED_FACE ( 'NONE', ( #20158 ), #11464, .T. ) ;
#18164 = PLANE ( 'NONE',  #6483 ) ;
#18165 = CARTESIAN_POINT ( 'NONE',  ( 55.71975233915209458, 77.37356315108866056, -16.50523346184714057 ) ) ;
#18166 = CARTESIAN_POINT ( 'NONE',  ( 221.0816127472251935, 31.79081672623770061, -13.95097276009444442 ) ) ;
#18167 = CARTESIAN_POINT ( 'NONE',  ( 172.0049095375684090, -3.964873019432352486, 0.9999999999999885647 ) ) ;
#18168 = EDGE_CURVE ( 'NONE', #17905, #10545, #17097, .T. ) ;
#18169 = CARTESIAN_POINT ( 'NONE',  ( 9.999999999999998224, 6.613092715395708453E-16, 5.400000000000001243 ) ) ;
#18170 = AXIS2_PLACEMENT_3D ( 'NONE', #3440, #20923, #4720 ) ;
#18171 = EDGE_CURVE ( 'NONE', #20000, #2929, #1192, .T. ) ;
#18172 = CARTESIAN_POINT ( 'NONE',  ( 49.86389338619021316, 127.5895726428436205, -12.50000000000000000 ) ) ;
#18173 = CARTESIAN_POINT ( 'NONE',  ( 0.03950703498306113587, 78.52235084885757033, -5.999488569659739312 ) ) ;
#18175 = VERTEX_POINT ( 'NONE', #12111 ) ;
#18174 = ORIENTED_EDGE ( 'NONE', *, *, #324, .F. ) ;
#18176 = DIRECTION ( 'NONE',  ( 0.000000000000000000, 0.000000000000000000, -1.000000000000000000 ) ) ;
#18177 = CARTESIAN_POINT ( 'NONE',  ( 31.00000000000000711, 65.00000000000000000, -12.50000000000000000 ) ) ;
#18178 = CARTESIAN_POINT ( 'NONE',  ( -33.23742054212824826, 77.39904134002362923, -4.045748805519247426 ) ) ;
#18179 = FACE_OUTER_BOUND ( 'NONE', #19347, .T. ) ;
#18180 = CARTESIAN_POINT ( 'NONE',  ( -29.99999999999999645, 5.000000000000000000, 4.650073815093233698 ) ) ;
#18181 = DIRECTION ( 'NONE',  ( -0.5171545105027488543, -0.2985792958513952544, 0.8021231927550450669 ) ) ;
#18182 = EDGE_LOOP ( 'NONE', ( #5650, #286, #14756, #6218, #3684, #7865 ) ) ;
#18183 = B_SPLINE_CURVE_WITH_KNOTS ( 'NONE', 3,
 ( #12463, #19130, #14168, #13842 ),
 .UNSPECIFIED., .F., .F.,
 ( 4, 4 ),
 ( 6.921599874492645062E-07, 0.0005666183822701121187 ),
 .UNSPECIFIED. ) ;
#18184 = CARTESIAN_POINT ( 'NONE',  ( 81.60718771731029619, 62.28998970175522487, -25.21698870735092513 ) ) ;
#18185 = CARTESIAN_POINT ( 'NONE',  ( -9.743283712094267912, 45.17557351322050607, -10.82820226318459333 ) ) ;
#18186 = EDGE_CURVE ( 'NONE', #17870, #13770, #14142, .T. ) ;
#18187 = ORIENTED_EDGE ( 'NONE', *, *, #19061, .F. ) ;
#18188 = LINE ( 'NONE', #13528, #8485 ) ;
#18189 = CARTESIAN_POINT ( 'NONE',  ( 1.482111447062408827, 53.96832415390036886, -2.310166060002879274 ) ) ;
#18190 = CARTESIAN_POINT ( 'NONE',  ( 1.494707070328831433, 76.40691198588817201, -2.756354051672949002 ) ) ;
#18191 = CARTESIAN_POINT ( 'NONE',  ( 172.3972143829816162, 19.35563505625646741, -9.000000000000007105 ) ) ;
#18192 = EDGE_CURVE ( 'NONE', #627, #7692, #4160, .T. ) ;
#18193 = CARTESIAN_POINT ( 'NONE',  ( -35.00000000000000000, 64.25000000000000000, 2.481238266578627449 ) ) ;
#18194 = CARTESIAN_POINT ( 'NONE',  ( 205.6925730159677244, 2.884952444891475842, -25.61390257072243770 ) ) ;
#18196 = ORIENTED_EDGE ( 'NONE', *, *, #16795, .F. ) ;
#18195 = EDGE_LOOP ( 'NONE', ( #6885, #12156, #5177 ) ) ;
#18197 = ORIENTED_EDGE ( 'NONE', *, *, #16041, .F. ) ;
#18198 = CARTESIAN_POINT ( 'NONE',  ( 204.7012550509497260, 2.055015527128745578, -24.96223045542551233 ) ) ;
#18199 = DIRECTION ( 'NONE',  ( 0.8660254037844355990, 0.5000000000000054401, 3.462567121588067547E-14 ) ) ;
#18200 = ORIENTED_EDGE ( 'NONE', *, *, #10984, .F. ) ;
#18201 = MECHANICAL_DESIGN_GEOMETRIC_PRESENTATION_REPRESENTATION (  '', ( #14167 ), #3630 ) ;
#18202 = PRODUCT ( 'Pin', 'Pin', '', ( #18891 ) ) ;
#18203 = CARTESIAN_POINT ( 'NONE',  ( 226.3850896897280904, 41.95196607254975874, -11.19450202347632128 ) ) ;
#18204 = DIRECTION ( 'NONE',  ( -0.5000000000000008882, 0.8660254037844381525, 0.000000000000000000 ) ) ;
#18205 = ORIENTED_EDGE ( 'NONE', *, *, #17776, .F. ) ;
#18206 = VECTOR ( 'NONE', #17389, 1000.000000000000114 ) ;
#18207 = EDGE_CURVE ( 'NONE', #5044, #17666, #20469, .T. ) ;
#18208 = DIRECTION ( 'NONE',  ( -0.8660254037844362651, -0.5000000000000043299, 0.000000000000000000 ) ) ;
#18209 = CARTESIAN_POINT ( 'NONE',  ( 218.8220856318716585, 37.62980918290750765, -16.74850582525157350 ) ) ;
#18210 = CARTESIAN_POINT ( 'NONE',  ( 198.5343390728978932, -1.505455072869313238, -12.62839849932143643 ) ) ;
#18211 = EDGE_CURVE ( 'NONE', #8949, #16469, #4785, .T. ) ;
#18212 = CARTESIAN_POINT ( 'NONE',  ( 179.0478494775924503, 57.83639716978969147, -18.91295074164678169 ) ) ;
#18213 = CARTESIAN_POINT ( 'NONE',  ( -33.48858877339391427, 53.74629247648528008, -2.576042629322002675 ) ) ;
#18214 = DIRECTION ( 'NONE',  ( 0.3841106397986914223, -0.6652991438591137063, 0.6401843996644798196 ) ) ;
#18215 = ORIENTED_EDGE ( 'NONE', *, *, #702, .F. ) ;
#18216 = EDGE_CURVE ( 'NONE', #18774, #4855, #983, .T. ) ;
#18217 = VECTOR ( 'NONE', #5733, 1000.000000000000114 ) ;
#18218 = CYLINDRICAL_SURFACE ( 'NONE', #14932, 12.47473710546057646 ) ;
#18219 = DIRECTION ( 'NONE',  ( -0.8660254037844363761, -0.5000000000000043299, 6.872020471724002955E-17 ) ) ;
#18221 = ORIENTED_EDGE ( 'NONE', *, *, #4874, .T. ) ;
#18220 = VERTEX_POINT ( 'NONE', #17198 ) ;
#18222 = CARTESIAN_POINT ( 'NONE',  ( 54.24218927016151781, 78.00150569360116037, -12.67188158619963900 ) ) ;
#18223 = ORIENTED_EDGE ( 'NONE', *, *, #3144, .F. ) ;
#18224 = B_SPLINE_CURVE_WITH_KNOTS ( 'NONE', 3,
 ( #15154, #18624, #16826, #10119 ),
 .UNSPECIFIED., .F., .F.,
 ( 4, 4 ),
 ( 1.578338979930638950E-06, 0.0006742291310329615386 ),
 .UNSPECIFIED. ) ;
#18225 = PLANE ( 'NONE',  #6097 ) ;
#18226 = CARTESIAN_POINT ( 'NONE',  ( -44.99469552244184456, 77.93309871596017047, 107.9872692538592531 ) ) ;
#18227 = EDGE_CURVE ( 'NONE', #305, #8941, #16655, .T. ) ;
#18228 = EDGE_CURVE ( 'NONE', #6893, #804, #874, .T. ) ;
#18229 = VECTOR ( 'NONE', #16791, 1000.000000000000000 ) ;
#18230 = ORIENTED_EDGE ( 'NONE', *, *, #2039, .F. ) ;
#18231 = DIRECTION ( 'NONE',  ( 0.5000000000000051070, -0.8660254037844355990, -1.942890293094023946E-16 ) ) ;
#18232 = EDGE_LOOP ( 'NONE', ( #4973, #9218, #14392, #11983 ) ) ;
#18233 = AXIS2_PLACEMENT_3D ( 'NONE', #15903, #1274, #19656 ) ;
#18234 = DIRECTION ( 'NONE',  ( -0.5000000000000049960, 0.8660254037844358210, -0.000000000000000000 ) ) ;
#18235 = VERTEX_POINT ( 'NONE', #2785 ) ;
#18236 = LINE ( 'NONE', #5283, #649 ) ;
#18237 = DIRECTION ( 'NONE',  ( -0.8660254037844378194, -0.5000000000000013323, -0.000000000000000000 ) ) ;
#18238 = ADVANCED_FACE ( 'NONE', ( #7425 ), #20576, .F. ) ;
#18239 = CARTESIAN_POINT ( 'NONE',  ( 205.8264633344831225, 9.596613037118636669, -14.00000000000005507 ) ) ;
#18240 = CARTESIAN_POINT ( 'NONE',  ( 7.999999999999998224, 0.000000000000000000, 0.000000000000000000 ) ) ;
#18241 = ORIENTED_EDGE ( 'NONE', *, *, #16223, .F. ) ;
#18242 = CARTESIAN_POINT ( 'NONE',  ( 196.3264911765913041, 4.642850816258196289, -8.609703802792473937 ) ) ;
#18243 = CARTESIAN_POINT ( 'NONE',  ( 218.9402551536602459, 37.01326326388927157, -16.94731950718122349 ) ) ;
#18244 = FACE_OUTER_BOUND ( 'NONE', #10319, .T. ) ;
#18245 = VECTOR ( 'NONE', #17385, 1000.000000000000114 ) ;
#18246 = EDGE_LOOP ( 'NONE', ( #1181, #19812, #10503, #2907 ) ) ;
#18247 = EDGE_CURVE ( 'NONE', #5922, #3941, #16179, .T. ) ;
#18248 = CARTESIAN_POINT ( 'NONE',  ( 81.38618934876433286, 61.60889898971228007, 0.05253686650109075373 ) ) ;
#18250 = LINE ( 'NONE', #13877, #15298 ) ;
#18249 = PRODUCT_DEFINITION_FORMATION_WITH_SPECIFIED_SOURCE ( 'ANY', '', #18202, .NOT_KNOWN. ) ;
#18251 = CARTESIAN_POINT ( 'NONE',  ( -12.45378882924321395, 69.43579287346189233, -3.531915534904312093 ) ) ;
#18252 = CARTESIAN_POINT ( 'NONE',  ( 78.21123729238362898, 52.55572853022376734, -8.703058536487507268 ) ) ;
#18254 = ORIENTED_EDGE ( 'NONE', *, *, #8069, .T. ) ;
#18253 = ORIENTED_EDGE ( 'NONE', *, *, #7420, .T. ) ;
#18255 = ORIENTED_EDGE ( 'NONE', *, *, #9720, .F. ) ;
#18256 = LINE ( 'NONE', #12008, #13420 ) ;
#18257 = AXIS2_PLACEMENT_3D ( 'NONE', #3239, #12903, #15989 ) ;
#18258 = ORIENTED_EDGE ( 'NONE', *, *, #10300, .F. ) ;
#18259 = CARTESIAN_POINT ( 'NONE',  ( 81.64154449522867196, 63.92558877093117076, -25.45657102965486018 ) ) ;
#18260 = LINE ( 'NONE', #16776, #10091 ) ;
#18261 = CARTESIAN_POINT ( 'NONE',  ( 159.9952905943348469, 46.83639716978958489, -29.00000000000006750 ) ) ;
#18262 = LINE ( 'NONE', #3728, #16747 ) ;
#18263 = ORIENTED_EDGE ( 'NONE', *, *, #6092, .F. ) ;
#18264 = CARTESIAN_POINT ( 'NONE',  ( 203.8052576239561802, 8.960718637850693113, -2.195132782454258358 ) ) ;
#18265 = CONICAL_SURFACE ( 'NONE', #5384, 4.509097725792825528, 0.5235987755983015912 ) ;
#18266 = CARTESIAN_POINT ( 'NONE',  ( 226.2189894626636431, 42.89261923747692862, -12.97935860811656816 ) ) ;
#18267 = CARTESIAN_POINT ( 'NONE',  ( 219.4414768585382944, 34.63161541676048927, -10.43865930680574827 ) ) ;
#18268 = ORIENTED_EDGE ( 'NONE', *, *, #19380, .T. ) ;
#18269 = FACE_OUTER_BOUND ( 'NONE', #12006, .T. ) ;
#18270 = DIRECTION ( 'NONE',  ( 0.8689290541588563510, 0.000000000000000000, -0.4949366614412345489 ) ) ;
#18271 = CARTESIAN_POINT ( 'NONE',  ( 46.51452848080092650, 183.3908428320656299, 11.00000000000001066 ) ) ;
#18272 = CARTESIAN_POINT ( 'NONE',  ( -13.41585758817372920, 79.99915570215716798, -12.30640999581525286 ) ) ;
#18273 = ORIENTED_EDGE ( 'NONE', *, *, #11551, .F. ) ;
#18274 = CIRCLE ( 'NONE', #8804, 3.619616396367202782 ) ;
#18275 = ADVANCED_FACE ( 'NONE', ( #15732 ), #7746, .T. ) ;
#18276 = CARTESIAN_POINT ( 'NONE',  ( 82.49529059433407951, 181.0703347563770365, 6.000000000000009770 ) ) ;
#18277 = CARTESIAN_POINT ( 'NONE',  ( 184.9952905943349606, 3.535126980567727450, -29.00000000000001066 ) ) ;
#18278 = DIRECTION ( 'NONE',  ( 0.8601696498176563122, 0.4966191788709776733, 0.1160929141252233648 ) ) ;
#18279 = CARTESIAN_POINT ( 'NONE',  ( 212.3629815419766373, 18.02552076297307337, -20.52105855319947025 ) ) ;
#18280 = CARTESIAN_POINT ( 'NONE',  ( -28.39160343344309112, 8.714752148389077746, 1.677005692623972699 ) ) ;
#18281 = DIRECTION ( 'NONE',  ( 0.5000000000000057732, -0.8660254037844353769, 0.000000000000000000 ) ) ;
#18282 = EDGE_LOOP ( 'NONE', ( #1696, #16489, #3320, #13163 ) ) ;
#18283 = EDGE_CURVE ( 'NONE', #10895, #3900, #15826, .T. ) ;
#18284 = CARTESIAN_POINT ( 'NONE',  ( 81.04710911000414342, 60.81400166747340563, -24.81806225219608208 ) ) ;
#18285 = CIRCLE ( 'NONE', #16591, 3.902363844300875240 ) ;
#18286 = CARTESIAN_POINT ( 'NONE',  ( -3.536038244605083314, 48.22321216239767949, -1.121469025438518452 ) ) ;
#18287 = CIRCLE ( 'NONE', #9139, 5.000000000000039968 ) ;
#18288 = EDGE_LOOP ( 'NONE', ( #17070, #18376, #11212, #6352, #11426 ) ) ;
#18289 = CARTESIAN_POINT ( 'NONE',  ( 202.3246710188176110, 25.20128250578996187, -15.50000755803645802 ) ) ;
#18290 = CARTESIAN_POINT ( 'NONE',  ( -3.238679877191993128, 60.93978609069553443, 1.964649670197885278 ) ) ;
#18291 = CARTESIAN_POINT ( 'NONE',  ( -6.040364182935697102, 79.85300711528874729, -10.39706325934435327 ) ) ;
#18292 = AXIS2_PLACEMENT_3D ( 'NONE', #10678, #14417, #1055 ) ;
#18293 = CARTESIAN_POINT ( 'NONE',  ( 205.5965122587965084, 9.994899983462953941, -14.00000000000005507 ) ) ;
#18294 = CYLINDRICAL_SURFACE ( 'NONE', #5395, 1.499999999999990896 ) ;
#18295 = CARTESIAN_POINT ( 'NONE',  ( 10.40000000000000568, 0.000000000000000000, 0.000000000000000000 ) ) ;
#18297 = ORIENTED_EDGE ( 'NONE', *, *, #13935, .F. ) ;
#18296 = ORIENTED_EDGE ( 'NONE', *, *, #5645, .F. ) ;
#18298 = ORIENTED_EDGE ( 'NONE', *, *, #12394, .F. ) ;
#18299 = CARTESIAN_POINT ( 'NONE',  ( 198.4225180578738161, 5.321943238602927728, -4.915515517929134326 ) ) ;
#18300 = DIRECTION ( 'NONE',  ( -0.5000000000000046629, 0.8660254037844359321, 0.000000000000000000 ) ) ;
#18301 = CIRCLE ( 'NONE', #3068, 11.00000000000002665 ) ;
#18302 = EDGE_CURVE ( 'NONE', #19734, #16889, #12537, .T. ) ;
#18303 = VERTEX_POINT ( 'NONE', #14248 ) ;
#18304 = ORIENTED_EDGE ( 'NONE', *, *, #13419, .F. ) ;
#18305 = EDGE_CURVE ( 'NONE', #15787, #11494, #16988, .T. ) ;
#18306 = CARTESIAN_POINT ( 'NONE',  ( 81.71672890644845211, 63.56720923707860749, 0.4227506902204759553 ) ) ;
#18307 = CARTESIAN_POINT ( 'NONE',  ( 205.9193846489986583, 10.18131044486005443, -11.67614332468980365 ) ) ;
#18308 = AXIS2_PLACEMENT_3D ( 'NONE', #17942, #8269, #233 ) ;
#18309 = CARTESIAN_POINT ( 'NONE',  ( 206.3904739784021842, 10.45329399600353959, -16.68557076349156176 ) ) ;
#18310 = ORIENTED_EDGE ( 'NONE', *, *, #2015, .F. ) ;
#18311 = B_SPLINE_CURVE_WITH_KNOTS ( 'NONE', 3,
 ( #3356, #19564, #11316, #16605 ),
 .UNSPECIFIED., .F., .F.,
 ( 4, 4 ),
 ( 8.130009260317344714E-07, 0.0008547987389088694586 ),
 .UNSPECIFIED. ) ;
#18312 = VECTOR ( 'NONE', #5452, 1000.000000000000000 ) ;
#18313 = CARTESIAN_POINT ( 'NONE',  ( 218.9002013747199555, 37.08263844404898180, -11.10922658182122902 ) ) ;
#18314 = DIRECTION ( 'NONE',  ( -0.8660254037844360431, -0.5000000000000044409, 5.976026924694052093E-17 ) ) ;
#18315 = EDGE_CURVE ( 'NONE', #18575, #2925, #12154, .T. ) ;
#18316 = ORIENTED_EDGE ( 'NONE', *, *, #17705, .F. ) ;
#18317 = EDGE_CURVE ( 'NONE', #3711, #15941, #6038, .T. ) ;
#18318 = DIRECTION ( 'NONE',  ( -0.8660254037844357100, -0.5000000000000051070, 0.000000000000000000 ) ) ;
#18319 = VECTOR ( 'NONE', #3766, 1000.000000000000114 ) ;
#18320 = CIRCLE ( 'NONE', #3749, 3.619616396367202782 ) ;
#18321 = CARTESIAN_POINT ( 'NONE',  ( 5.000000000000004441, 7.027796151710827388, -4.057500000000009877 ) ) ;
#18322 = CARTESIAN_POINT ( 'NONE',  ( -31.60861962881361720, 50.39374029569145108, -9.070721203488703921 ) ) ;
#18323 = DIRECTION ( 'NONE',  ( -0.5000000000000056621, 0.8660254037844352659, 0.000000000000000000 ) ) ;
#18324 = VERTEX_POINT ( 'NONE', #12741 ) ;
#18325 = CARTESIAN_POINT ( 'NONE',  ( 218.1588199976357032, 38.33690813194773739, -14.17836540244684684 ) ) ;
#18326 = CIRCLE ( 'NONE', #9502, 4.172000000000029907 ) ;
#18327 = CARTESIAN_POINT ( 'NONE',  ( 227.5713637699006426, 40.55023822649137344, -10.17395310825081189 ) ) ;
#18328 = EDGE_CURVE ( 'NONE', #12799, #17970, #3294, .T. ) ;
#18330 = ORIENTED_EDGE ( 'NONE', *, *, #18228, .T. ) ;
#18329 = ORIENTED_EDGE ( 'NONE', *, *, #16940, .F. ) ;
#18331 = CARTESIAN_POINT ( 'NONE',  ( 55.32129083036254968, 77.54301705067358341, -15.95188330757220996 ) ) ;
#18332 = VERTEX_POINT ( 'NONE', #19106 ) ;
#18333 = VERTEX_POINT ( 'NONE', #1403 ) ;
#18334 = FACE_BOUND ( 'NONE', #4741, .T. ) ;
#18335 = DIRECTION ( 'NONE',  ( 0.8660254037844370423, 0.5000000000000026645, -0.000000000000000000 ) ) ;
#18336 = ADVANCED_FACE ( 'NONE', ( #14666, #6454 ), #12850, .T. ) ;
#18337 = CIRCLE ( 'NONE', #17327, 5.000000000000001776 ) ;
#18338 = ORIENTED_EDGE ( 'NONE', *, *, #20482, .F. ) ;
#18339 = DIRECTION ( 'NONE',  ( -0.8660254037844380415, -0.5000000000000014433, -0.000000000000000000 ) ) ;
#18340 = CIRCLE ( 'NONE', #748, 5.000000000000039968 ) ;
#18341 = VECTOR ( 'NONE', #2175, 1000.000000000000000 ) ;
#18342 = ADVANCED_FACE ( 'NONE', ( #11352 ), #6558, .T. ) ;
#18343 = VECTOR ( 'NONE', #4279, 1000.000000000000000 ) ;
#18344 = LINE ( 'NONE', #6877, #5533 ) ;
#18345 = ORIENTED_EDGE ( 'NONE', *, *, #13388, .F. ) ;
#18346 = FACE_BOUND ( 'NONE', #5551, .T. ) ;
#18347 = DIRECTION ( 'NONE',  ( 0.5000000000000041078, -0.8660254037844362651, 0.000000000000000000 ) ) ;
#18348 = CARTESIAN_POINT ( 'NONE',  ( 214.9166615741016244, 8.725703323795450217, -24.01557619556987078 ) ) ;
#18349 = DIRECTION ( 'NONE',  ( 1.000000000000000000, 2.509104035652853150E-14, 0.000000000000000000 ) ) ;
#18350 = EDGE_CURVE ( 'NONE', #7973, #13380, #3506, .T. ) ;
#18351 = CARTESIAN_POINT ( 'NONE',  ( -28.93885174497882673, 72.78546382685756555, 0.3359787457726054472 ) ) ;
#18352 = VECTOR ( 'NONE', #16158, 1000.000000000000000 ) ;
#18353 = CARTESIAN_POINT ( 'NONE',  ( 218.4367820612134494, 37.88530424025100984, -12.10162843130809840 ) ) ;
#18354 = LINE ( 'NONE', #2242, #7842 ) ;
#18355 = ADVANCED_FACE ( 'NONE', ( #14352 ), #124, .F. ) ;
#18356 = VERTEX_POINT ( 'NONE', #14556 ) ;
#18357 = AXIS2_PLACEMENT_3D ( 'NONE', #1287, #2771, #19189 ) ;
#18358 = AXIS2_PLACEMENT_3D ( 'NONE', #6282, #3325, #12776 ) ;
#18359 = CARTESIAN_POINT ( 'NONE',  ( 64.99529059433395162, 211.3812238888322952, 16.00000000000001066 ) ) ;
#18360 = CIRCLE ( 'NONE', #10912, 12.47473710546057823 ) ;
#18361 = DIRECTION ( 'NONE',  ( -0.5000000000000049960, 0.8660254037844357100, -0.000000000000000000 ) ) ;
#18362 = CYLINDRICAL_SURFACE ( 'NONE', #3559, 5.000000000000001776 ) ;
#18363 = EDGE_CURVE ( 'NONE', #11167, #8949, #12826, .T. ) ;
#18365 = VERTEX_POINT ( 'NONE', #6154 ) ;
#18364 = ORIENTED_EDGE ( 'NONE', *, *, #17969, .T. ) ;
#18366 =( LENGTH_UNIT ( ) NAMED_UNIT ( * ) SI_UNIT ( .MILLI., .METRE. ) );
#18367 = CARTESIAN_POINT ( 'NONE',  ( 209.3909370991932235, 3.422763374394450775, -14.00000000000005507 ) ) ;
#18368 = ORIENTED_EDGE ( 'NONE', *, *, #10790, .T. ) ;
#18369 = CARTESIAN_POINT ( 'NONE',  ( 81.06711713768373784, 65.00000000000000000, -25.50000000000000000 ) ) ;
#18370 = EDGE_CURVE ( 'NONE', #18220, #10039, #20920, .T. ) ;
#18371 = CARTESIAN_POINT ( 'NONE',  ( -21.54135399647558202, 79.97447990077583313, -11.55951008316331574 ) ) ;
#18372 = CIRCLE ( 'NONE', #18711, 3.619616396367202782 ) ;
#18373 = CARTESIAN_POINT ( 'NONE',  ( 221.7170026686113147, 32.20379548820332616, -14.53509620734056540 ) ) ;
#18374 = LINE ( 'NONE', #13710, #346 ) ;
#18375 = AXIS2_PLACEMENT_3D ( 'NONE', #13973, #20510, #12274 ) ;
#18376 = ORIENTED_EDGE ( 'NONE', *, *, #1211, .T. ) ;
#18377 = DIRECTION ( 'NONE',  ( 0.5000000000000044409, -0.8660254037844360431, 0.000000000000000000 ) ) ;
#18378 = DIRECTION ( 'NONE',  ( -0.6299240516454519545, -0.3636868207865264768, 0.6862416378687370422 ) ) ;
#18379 = CYLINDRICAL_SURFACE ( 'NONE', #12464, 12.47473710546057646 ) ;
#18380 = PRODUCT ( 'Rear Drill Bit Retaining Pin', 'Rear Drill Bit Retaining Pin', '', ( #2882 ) ) ;
#18381 = VERTEX_POINT ( 'NONE', #17825 ) ;
#18382 = CARTESIAN_POINT ( 'NONE',  ( 105.0828820505367531, 187.4071680446163555, 11.00000000000001066 ) ) ;
#18383 = CARTESIAN_POINT ( 'NONE',  ( 197.6158938898029191, 5.210277915641273516, -6.188753603159779182 ) ) ;
#18384 = CARTESIAN_POINT ( 'NONE',  ( 198.7027818574981666, 10.13880079795527323, -24.25943249057081630 ) ) ;
#18385 = CARTESIAN_POINT ( 'NONE',  ( -6.484348779698995813, 79.99999999992091659, -8.118105310438910038 ) ) ;
#18386 = AXIS2_PLACEMENT_3D ( 'NONE', #7181, #12392, #12289 ) ;
#18387 = ORIENTED_EDGE ( 'NONE', *, *, #18216, .T. ) ;
#18388 = VERTEX_POINT ( 'NONE', #12646 ) ;
#18389 = FACE_OUTER_BOUND ( 'NONE', #7223, .T. ) ;
#18390 = CYLINDRICAL_SURFACE ( 'NONE', #12579, 3.902363844300889451 ) ;
#18391 = CARTESIAN_POINT ( 'NONE',  ( 227.6158839122614097, 40.47312707796264419, -10.49174204642374697 ) ) ;
#18392 = CARTESIAN_POINT ( 'NONE',  ( 5.000000000000004441, 4.685197434473814759, -6.938893903907228378E-15 ) ) ;
#18393 = CARTESIAN_POINT ( 'NONE',  ( -25.99999999999998934, 9.999999999999994671, 7.500000000000008882 ) ) ;
#18394 = CARTESIAN_POINT ( 'NONE',  ( 197.9670180026625417, -1.060177954843255499, -16.89203719259486647 ) ) ;
#18395 = VERTEX_POINT ( 'NONE', #4675 ) ;
#18396 = CARTESIAN_POINT ( 'NONE',  ( 79.48084484536077809, 58.16953689576122599, -23.57162899958074931 ) ) ;
#18397 = CARTESIAN_POINT ( 'NONE',  ( 217.4723034443702545, 9.685982978710988789, -7.343163769975822319 ) ) ;
#18398 = AXIS2_PLACEMENT_3D ( 'NONE', #19262, #4730, #19360 ) ;
#18399 = ORIENTED_EDGE ( 'NONE', *, *, #18559, .F. ) ;
#18400 = DIRECTION ( 'NONE',  ( -1.000000000000000000, -0.000000000000000000, -0.000000000000000000 ) ) ;
#18401 = CARTESIAN_POINT ( 'NONE',  ( -0.1451441909484942616, 63.40414104109810722, 2.432067769318205119 ) ) ;
#18402 = LINE ( 'NONE', #3870, #7552 ) ;
#18403 = CARTESIAN_POINT ( 'NONE',  ( 77.62926519054970242, 189.4985379866525648, 11.00000000000001066 ) ) ;
#18404 = CARTESIAN_POINT ( 'NONE',  ( 96.88087538439037871, 198.6134603144003563, 11.00000000000000888 ) ) ;
#18405 = FACE_OUTER_BOUND ( 'NONE', #17895, .T. ) ;
#18407 = VERTEX_POINT ( 'NONE', #3192 ) ;
#18406 = ORIENTED_EDGE ( 'NONE', *, *, #16298, .F. ) ;
#18408 = ORIENTED_EDGE ( 'NONE', *, *, #13170, .F. ) ;
#18409 = CARTESIAN_POINT ( 'NONE',  ( 213.4477085251712936, 18.65178817871777994, -9.972943347742015519 ) ) ;
#18410 = DIRECTION ( 'NONE',  ( -1.000000000000000000, -0.000000000000000000, -0.000000000000000000 ) ) ;
#18411 = VERTEX_POINT ( 'NONE', #11143 ) ;
#18412 = ORIENTED_EDGE ( 'NONE', *, *, #15780, .F. ) ;
#18413 = ADVANCED_FACE ( 'NONE', ( #17619 ), #9645, .F. ) ;
#18414 = CARTESIAN_POINT ( 'NONE',  ( 205.5965122587965084, 9.994899983462953941, -14.00000000000005507 ) ) ;
#18415 = CARTESIAN_POINT ( 'NONE',  ( 32.36389338619004263, 157.9004617752989930, 4.000000000000000000 ) ) ;
#18416 = CARTESIAN_POINT ( 'NONE',  ( 5.000000000000000000, -2.342598717236899386, 4.057500000000001883 ) ) ;
#18417 = CIRCLE ( 'NONE', #9253, 4.999999999999978684 ) ;
#18418 = CIRCLE ( 'NONE', #16726, 3.619616396367202782 ) ;
#18419 = EDGE_LOOP ( 'NONE', ( #8956, #12282, #13852, #13904 ) ) ;
#18420 = CARTESIAN_POINT ( 'NONE',  ( 217.6445881269244182, 37.74391799546369697, -11.31761084191174938 ) ) ;
#18421 = CARTESIAN_POINT ( 'NONE',  ( 203.9637611243273057, 8.521181414665040421, -26.28791492288515386 ) ) ;
#18422 = ORIENTED_EDGE ( 'NONE', *, *, #18738, .F. ) ;
#18423 = LINE ( 'NONE', #3892, #20623 ) ;
#18424 = ADVANCED_FACE ( 'NONE', ( #17929 ), #16139, .F. ) ;
#18425 = CARTESIAN_POINT ( 'NONE',  ( 196.7772661521197222, -0.8746956702846723219, -14.00000000000005507 ) ) ;
#18426 = CARTESIAN_POINT ( 'NONE',  ( -30.38872702552290761, 50.11721826652506451, -10.60405991245520418 ) ) ;
#18427 = CARTESIAN_POINT ( 'NONE',  ( 210.5759555690915192, 16.99378083647902216, -24.58554911381534325 ) ) ;
#18428 = VECTOR ( 'NONE', #11616, 1000.000000000000114 ) ;
#18429 = DIRECTION ( 'NONE',  ( 0.000000000000000000, 0.000000000000000000, 1.000000000000000000 ) ) ;
#18430 = DIRECTION ( 'NONE',  ( 0.5000000000000054401, -0.8660254037844354880, 0.000000000000000000 ) ) ;
#18432 = ORIENTED_EDGE ( 'NONE', *, *, #11362, .T. ) ;
#18431 = ORIENTED_EDGE ( 'NONE', *, *, #16901, .T. ) ;
#18433 = CARTESIAN_POINT ( 'NONE',  ( 58.64342261736307194, 85.44810595174396894, -13.47428068817142943 ) ) ;
#18434 = ADVANCED_FACE ( 'NONE', ( #4885 ), #3389, .T. ) ;
#18435 = ORIENTED_EDGE ( 'NONE', *, *, #11493, .F. ) ;
#18436 = ORIENTED_EDGE ( 'NONE', *, *, #1148, .F. ) ;
#18437 = EDGE_CURVE ( 'NONE', #15696, #3474, #11258, .T. ) ;
#18438 = ORIENTED_EDGE ( 'NONE', *, *, #19135, .F. ) ;
#18439 = DIRECTION ( 'NONE',  ( -0.5000000000000049960, 0.8660254037844357100, -0.000000000000000000 ) ) ;
#18440 = DIRECTION ( 'NONE',  ( 0.000000000000000000, 0.000000000000000000, 1.000000000000000000 ) ) ;
#18441 = VERTEX_POINT ( 'NONE', #20879 ) ;
#18442 = PLANE ( 'NONE',  #10032 ) ;
#18443 = ORIENTED_EDGE ( 'NONE', *, *, #7030, .T. ) ;
#18444 = AXIS2_PLACEMENT_3D ( 'NONE', #17119, #12253, #4292 ) ;
#18445 = DIRECTION ( 'NONE',  ( 0.000000000000000000, 8.673617379884020681E-16, -1.000000000000000000 ) ) ;
#18446 = CARTESIAN_POINT ( 'NONE',  ( 204.7255155853154918, 2.069022353175566931, -3.025685634606110952 ) ) ;
#18447 = CARTESIAN_POINT ( 'NONE',  ( 54.65554463217808490, 249.2901892326410689, -13.99999999999998046 ) ) ;
#18448 = B_SPLINE_CURVE_WITH_KNOTS ( 'NONE', 3,
 ( #2808, #17112, #17009, #15846, #1212, #9140, #7663, #2601, #13833, #895, #19024, #18806, #10961, #9042, #6448, #4497, #1111, #15544, #1002, #10735 ),
 .UNSPECIFIED., .F., .F.,
 ( 4, 2, 2, 2, 2, 2, 2, 2, 2, 4 ),
 ( 0.000000000000000000, 0.0009877350076376205726, 0.001975470015275241145, 0.002963205022912861718, 0.003950940030550482290, 0.004938675038188102863, 0.005926410045825723436, 0.006420277549644531553, 0.006914145053463339671, 0.007901880061100961111 ),
 .UNSPECIFIED. ) ;
#18449 = PLANE ( 'NONE',  #17335 ) ;
#18451 = DIRECTION ( 'NONE',  ( 0.8660254037844370423, 0.5000000000000027756, 0.000000000000000000 ) ) ;
#18450 = B_SPLINE_CURVE_WITH_KNOTS ( 'NONE', 3,
 ( #696, #15450, #806, #7152 ),
 .UNSPECIFIED., .F., .F.,
 ( 4, 4 ),
 ( 1.854400302406807709E-06, 0.0008558401382792385015 ),
 .UNSPECIFIED. ) ;
#18452 = CARTESIAN_POINT ( 'NONE',  ( 4.000000000000000000, 0.000000000000000000, 3.047499999999999876 ) ) ;
#18453 = EDGE_CURVE ( 'NONE', #12613, #4251, #18686, .T. ) ;
#18454 = CARTESIAN_POINT ( 'NONE',  ( 216.2725394319739110, 15.91768827161142674, -14.00000000000005507 ) ) ;
#18455 = DIRECTION ( 'NONE',  ( -0.8660254037844380415, -0.5000000000000014433, -0.000000000000000000 ) ) ;
#18456 = CARTESIAN_POINT ( 'NONE',  ( 217.7814145706309432, 37.50692764314506178, -12.10162843130809662 ) ) ;
#18457 = VERTEX_POINT ( 'NONE', #6355 ) ;
#18458 = CARTESIAN_POINT ( 'NONE',  ( 80.19404268355357601, 59.28982122532673316, -0.8110594018112234904 ) ) ;
#18459 = EDGE_CURVE ( 'NONE', #2018, #11054, #8154, .T. ) ;
#18460 = AXIS2_PLACEMENT_3D ( 'NONE', #15626, #5625, #18898 ) ;
#18461 = ORIENTED_EDGE ( 'NONE', *, *, #8727, .F. ) ;
#18462 = CARTESIAN_POINT ( 'NONE',  ( 207.8527399996651184, 15.42153159440924881, -3.125199447383529172 ) ) ;
#18463 = CARTESIAN_POINT ( 'NONE',  ( 64.99529059433392320, 211.3812238888322952, 11.00000000000001066 ) ) ;
#18464 = ADVANCED_FACE ( 'NONE', ( #19709 ), #2232, .F. ) ;
#18465 = VERTEX_POINT ( 'NONE', #16649 ) ;
#18466 = EDGE_CURVE ( 'NONE', #11090, #4169, #15900, .T. ) ;
#18467 = DIRECTION ( 'NONE',  ( 0.000000000000000000, 0.000000000000000000, 1.000000000000000000 ) ) ;
#18468 = DIRECTION ( 'NONE',  ( -0.8660254037844360431, -0.5000000000000043299, 0.000000000000000000 ) ) ;
#18469 = EDGE_CURVE ( 'NONE', #19987, #15362, #9767, .T. ) ;
#18470 = ORIENTED_EDGE ( 'NONE', *, *, #1844, .F. ) ;
#18471 = DIRECTION ( 'NONE',  ( -0.8660254037844350439, -0.5000000000000061062, 0.000000000000000000 ) ) ;
#18472 = AXIS2_PLACEMENT_3D ( 'NONE', #2205, #11746, #7066 ) ;
#18473 = CARTESIAN_POINT ( 'NONE',  ( -23.80213736597611884, 79.89664383654029223, -10.58772689523770083 ) ) ;
#18474 = DIRECTION ( 'NONE',  ( 0.5000000000000044409, -0.8660254037844360431, -4.006172263299080068E-16 ) ) ;
#18475 = DIRECTION ( 'NONE',  ( 0.5000000000000049960, -0.8660254037844358210, 0.000000000000000000 ) ) ;
#18476 = DIRECTION ( 'NONE',  ( -0.4272097022732502247, 0.7399489098236364804, 0.5195839500354230145 ) ) ;
#18477 = B_SPLINE_CURVE_WITH_KNOTS ( 'NONE', 3,
 ( #12233, #9133, #12345, #18799 ),
 .UNSPECIFIED., .F., .F.,
 ( 4, 4 ),
 ( 3.618634372173678480E-05, 0.0006021125660084806694 ),
 .UNSPECIFIED. ) ;
#18478 = CONICAL_SURFACE ( 'NONE', #8650, 10.26794919243114634, 1.047197551196596965 ) ;
#18479 = EDGE_CURVE ( 'NONE', #5664, #13156, #2010, .T. ) ;
#18480 = DIRECTION ( 'NONE',  ( -0.5000000000000045519, 0.8660254037844360431, 0.000000000000000000 ) ) ;
#18481 = CARTESIAN_POINT ( 'NONE',  ( -27.50180796992659182, 64.24999999999997158, 4.917728941844616841 ) ) ;
#18482 = ORIENTED_EDGE ( 'NONE', *, *, #6886, .F. ) ;
#18483 = CARTESIAN_POINT ( 'NONE',  ( 199.2144802262915846, 21.04890371929339921, -14.00000000000005507 ) ) ;
#18484 = DIRECTION ( 'NONE',  ( -0.2961981327260175823, -0.1710100716628329964, 0.9396926207859105373 ) ) ;
#18485 = AXIS2_PLACEMENT_3D ( 'NONE', #6708, #17977, #6606 ) ;
#18486 = CARTESIAN_POINT ( 'NONE',  ( 227.9553588074475954, 39.88513931160571957, -14.00000000000005507 ) ) ;
#18487 = EDGE_CURVE ( 'NONE', #8377, #1231, #16858, .T. ) ;
#18488 = CARTESIAN_POINT ( 'NONE',  ( -105.2819322368043515, 182.3536557531674873, -1.028642961561239307E-12 ) ) ;
#18489 = EDGE_CURVE ( 'NONE', #5298, #12547, #19601, .T. ) ;
#18491 = ORIENTED_EDGE ( 'NONE', *, *, #13316, .T. ) ;
#18490 = ORIENTED_EDGE ( 'NONE', *, *, #5637, .F. ) ;
#18492 = ORIENTED_EDGE ( 'NONE', *, *, #11932, .F. ) ;
#18493 = CIRCLE ( 'NONE', #18826, 4.057500000000029416 ) ;
#18494 = DIRECTION ( 'NONE',  ( -0.5000000000000052180, 0.8660254037844355990, 0.000000000000000000 ) ) ;
#18495 = DIRECTION ( 'NONE',  ( 0.000000000000000000, -6.938893903907177533E-18, -1.000000000000000000 ) ) ;
#18496 = EDGE_CURVE ( 'NONE', #8008, #12002, #2133, .T. ) ;
#18497 = CARTESIAN_POINT ( 'NONE',  ( 79.54876660668207933, 50.01490354004885575, -15.87845277340799477 ) ) ;
#18498 = EDGE_CURVE ( 'NONE', #14657, #9834, #15082, .T. ) ;
#18499 = CARTESIAN_POINT ( 'NONE',  ( -28.48655238447041071, 8.589452128384102991, 0.6702984623187877578 ) ) ;
#18500 =( NAMED_UNIT ( * ) SI_UNIT ( $, .STERADIAN. ) SOLID_ANGLE_UNIT ( ) );
#18501 = LINE ( 'NONE', #12037, #829 ) ;
#18502 = VERTEX_POINT ( 'NONE', #6769 ) ;
#18503 = CARTESIAN_POINT ( 'NONE',  ( 82.91256048669795575, 62.99717322904664485, -25.49106880622069937 ) ) ;
#18504 = AXIS2_PLACEMENT_3D ( 'NONE', #17953, #3418, #9766 ) ;
#18505 = FACE_OUTER_BOUND ( 'NONE', #892, .T. ) ;
#18506 = EDGE_CURVE ( 'NONE', #14336, #16764, #1748, .T. ) ;
#18507 = ORIENTED_EDGE ( 'NONE', *, *, #4043, .F. ) ;
#18508 = AXIS2_PLACEMENT_3D ( 'NONE', #17483, #2959, #1368 ) ;
#18509 = CARTESIAN_POINT ( 'NONE',  ( 201.8425266500695727, 26.45120969970218283, -14.48650656672420389 ) ) ;
#18510 = DIRECTION ( 'NONE',  ( -0.8137976813493682515, -0.4698463103929579887, 0.3420201433256764290 ) ) ;
#18511 = CARTESIAN_POINT ( 'NONE',  ( 228.3010954329995741, 39.28630591011256001, -10.44704522969155391 ) ) ;
#18512 = CARTESIAN_POINT ( 'NONE',  ( 34.99529059433362477, 263.3427481158986438, -28.99999999999998934 ) ) ;
#18513 = CARTESIAN_POINT ( 'NONE',  ( 199.3895759864363413, 6.411323655772897645, -23.60546391700144397 ) ) ;
#18515 = VERTEX_POINT ( 'NONE', #14870 ) ;
#18514 = ORIENTED_EDGE ( 'NONE', *, *, #4022, .F. ) ;
#18516 = VERTEX_POINT ( 'NONE', #18031 ) ;
#18517 = DIRECTION ( 'NONE',  ( 0.8660254037844355990, 0.5000000000000051070, -1.748523119690306661E-16 ) ) ;
#18518 = EDGE_CURVE ( 'NONE', #18726, #2303, #17588, .T. ) ;
#18519 = DIRECTION ( 'NONE',  ( -0.8660254037844360431, -0.5000000000000045519, -4.336808689942050277E-16 ) ) ;
#18520 = ORIENTED_EDGE ( 'NONE', *, *, #18437, .F. ) ;
#18521 = ORIENTED_EDGE ( 'NONE', *, *, #18722, .T. ) ;
#18522 = CARTESIAN_POINT ( 'NONE',  ( 81.71881349453083487, 62.89257827863775674, 0.3300630968703215373 ) ) ;
#18523 = DIRECTION ( 'NONE',  ( 0.8660254037844372643, 0.5000000000000027756, -0.000000000000000000 ) ) ;
#18524 = DIRECTION ( 'NONE',  ( 0.000000000000000000, -6.938893903907177533E-18, -1.000000000000000000 ) ) ;
#18525 = FACE_OUTER_BOUND ( 'NONE', #19803, .T. ) ;
#18526 = VECTOR ( 'NONE', #5223, 1000.000000000000227 ) ;
#18527 = DIRECTION ( 'NONE',  ( -0.4999999999999995004, 0.8660254037844390407, 0.000000000000000000 ) ) ;
#18528 = CIRCLE ( 'NONE', #13792, 4.172000000000029907 ) ;
#18529 = EDGE_CURVE ( 'NONE', #2046, #8261, #13263, .T. ) ;
#18530 = ORIENTED_EDGE ( 'NONE', *, *, #6963, .T. ) ;
#18531 = CARTESIAN_POINT ( 'NONE',  ( -15.99999999999999289, 5.000000000000000000, 0.000000000000000000 ) ) ;
#18532 = ADVANCED_FACE ( 'NONE', ( #18346, #222 ), #6985, .F. ) ;
#18533 = FACE_OUTER_BOUND ( 'NONE', #6112, .T. ) ;
#18534 = CARTESIAN_POINT ( 'NONE',  ( -15.53172565362767266, 50.47638478530413408, -16.25028014708374613 ) ) ;
#18535 = DIRECTION ( 'NONE',  ( 0.8660254037844370423, 0.5000000000000026645, -0.000000000000000000 ) ) ;
#18536 = DIRECTION ( 'NONE',  ( -0.4814586436739069497, 0.8339108325863940907, 0.2697967711570114502 ) ) ;
#18537 = CARTESIAN_POINT ( 'NONE',  ( -27.30844811143078132, 63.47441656769112228, 5.326305501724396763 ) ) ;
#18538 = AXIS2_PLACEMENT_3D ( 'NONE', #409, #17796, #6857 ) ;
#18540 = EDGE_LOOP ( 'NONE', ( #17130, #503 ) ) ;
#18539 = EDGE_LOOP ( 'NONE', ( #10359, #12975, #13845, #3415 ) ) ;
#18541 = APPLICATION_CONTEXT ( 'automotive_design' ) ;
#18542 = B_SPLINE_CURVE_WITH_KNOTS ( 'NONE', 3,
 ( #2605, #7944, #11037, #14447 ),
 .UNSPECIFIED., .F., .F.,
 ( 4, 4 ),
 ( 8.179433511367805316E-07, 0.0004528711851310280559 ),
 .UNSPECIFIED. ) ;
#18543 = CARTESIAN_POINT ( 'NONE',  ( 58.06035037439094282, 76.37624806333415961, -18.80372476195067932 ) ) ;
#18544 = VECTOR ( 'NONE', #2290, 1000.000000000000000 ) ;
#18545 = ORIENTED_EDGE ( 'NONE', *, *, #13824, .F. ) ;
#18546 = ORIENTED_EDGE ( 'NONE', *, *, #6429, .F. ) ;
#18547 = CARTESIAN_POINT ( 'NONE',  ( 199.2144802262915846, 21.04890371929339921, -14.00000000000005507 ) ) ;
#18548 = CARTESIAN_POINT ( 'NONE',  ( 226.5371121300225923, 42.34161461457158993, -11.75146085096529269 ) ) ;
#18549 = EDGE_CURVE ( 'NONE', #14915, #2174, #19684, .T. ) ;
#18550 = ORIENTED_EDGE ( 'NONE', *, *, #15491, .F. ) ;
#18551 = ORIENTED_EDGE ( 'NONE', *, *, #3433, .T. ) ;
#18552 = DIRECTION ( 'NONE',  ( 0.000000000000000000, 0.000000000000000000, -1.000000000000000000 ) ) ;
#18553 = ORIENTED_EDGE ( 'NONE', *, *, #17677, .F. ) ;
#18554 = CARTESIAN_POINT ( 'NONE',  ( 208.8107687779841228, 4.427644383670616079, -14.00000000000005507 ) ) ;
#18555 = LINE ( 'NONE', #4021, #12661 ) ;
#18556 = VECTOR ( 'NONE', #12482, 1000.000000000000000 ) ;
#18557 = DIRECTION ( 'NONE',  ( 0.000000000000000000, 1.000000000000000000, 0.000000000000000000 ) ) ;
#18558 = VECTOR ( 'NONE', #6696, 1000.000000000000114 ) ;
#18559 = EDGE_CURVE ( 'NONE', #16469, #9266, #18236, .T. ) ;
#18560 = DIRECTION ( 'NONE',  ( 0.000000000000000000, 0.5000000000000009992, 0.8660254037844381525 ) ) ;
#18561 = DIRECTION ( 'NONE',  ( -0.3654179821390599048, 0.6329225110641439889, -0.6825531432186626724 ) ) ;
#18562 = CARTESIAN_POINT ( 'NONE',  ( 30.10683012259193703, 0.000000000000000000, 0.000000000000000000 ) ) ;
#18563 = CARTESIAN_POINT ( 'NONE',  ( -27.98480658401470578, 74.73312780907578201, 3.553696893467978679 ) ) ;
#18564 = CARTESIAN_POINT ( 'NONE',  ( 177.1791022559528983, 56.75747545832872731, -14.00000000000006395 ) ) ;
#18565 = FACE_OUTER_BOUND ( 'NONE', #10044, .T. ) ;
#18566 = ORIENTED_EDGE ( 'NONE', *, *, #20937, .F. ) ;
#18567 = CARTESIAN_POINT ( 'NONE',  ( 78.57013627436289482, 56.82968174286880014, -2.376451016691543572 ) ) ;
#18568 = MECHANICAL_DESIGN_GEOMETRIC_PRESENTATION_REPRESENTATION (  '', ( #11120 ), #1978 ) ;
#18569 = ORIENTED_EDGE ( 'NONE', *, *, #15881, .T. ) ;
#18570 = LINE ( 'NONE', #18462, #19982 ) ;
#18571 = CARTESIAN_POINT ( 'NONE',  ( 81.10655718899693056, 54.43739570253208626, -2.927339837274431922 ) ) ;
#18572 = AXIS2_PLACEMENT_3D ( 'NONE', #5835, #15619, #8706 ) ;
#18573 = DIRECTION ( 'NONE',  ( 1.000000000000000000, 0.000000000000000000, 0.000000000000000000 ) ) ;
#18574 = CARTESIAN_POINT ( 'NONE',  ( 219.7433394806820672, 35.59225560066523286, -17.54145750504257961 ) ) ;
#18575 = VERTEX_POINT ( 'NONE', #11989 ) ;
#18576 = CARTESIAN_POINT ( 'NONE',  ( 75.39104360666324567, 52.47794215086291558, -8.991240694413738410 ) ) ;
#18577 = CARTESIAN_POINT ( 'NONE',  ( 203.5058955171470814, 23.52655349267333307, -2.551678190571530891 ) ) ;
#18578 = LINE ( 'NONE', #6047, #5575 ) ;
#18579 = FACE_OUTER_BOUND ( 'NONE', #8330, .T. ) ;
#18580 = VERTEX_POINT ( 'NONE', #16437 ) ;
#18581 = ADVANCED_FACE ( 'NONE', ( #11669 ), #13581, .F. ) ;
#18582 = EDGE_CURVE ( 'NONE', #4855, #7191, #19920, .T. ) ;
#18583 = DIRECTION ( 'NONE',  ( 0.1017280065263165834, -0.1761980758562760596, 0.9790840876823235783 ) ) ;
#18584 = CARTESIAN_POINT ( 'NONE',  ( 59.87106025315629410, 220.2566511894378039, 48.96815749462643197 ) ) ;
#18585 = DIRECTION ( 'NONE',  ( 0.8660254037844368202, 0.5000000000000031086, -0.000000000000000000 ) ) ;
#18586 = VERTEX_POINT ( 'NONE', #2762 ) ;
#18587 = LINE ( 'NONE', #15427, #18979 ) ;
#18588 = CARTESIAN_POINT ( 'NONE',  ( 197.5788830768223647, 5.011893035631070248, -6.091045511236785615 ) ) ;
#18589 = ADVANCED_FACE ( 'NONE', ( #10475 ), #14117, .T. ) ;
#18590 = CARTESIAN_POINT ( 'NONE',  ( 195.9724448824713932, 4.438442093042461956, -18.06789442459577089 ) ) ;
#18591 = DIRECTION ( 'NONE',  ( -0.000000000000000000, -0.000000000000000000, 1.000000000000000000 ) ) ;
#18593 = ORIENTED_EDGE ( 'NONE', *, *, #4968, .F. ) ;
#18592 = EDGE_LOOP ( 'NONE', ( #12640, #9094, #5292 ) ) ;
#18594 = CIRCLE ( 'NONE', #12167, 4.999999999999989342 ) ;
#18595 = CARTESIAN_POINT ( 'NONE',  ( 218.9914638623158396, 11.07829152179047760, -11.13829696442610029 ) ) ;
#18596 = CARTESIAN_POINT ( 'NONE',  ( 198.9132435853529728, 11.57066088650059932, -14.00000000000004974 ) ) ;
#18597 = ORIENTED_EDGE ( 'NONE', *, *, #1132, .F. ) ;
#18598 = CARTESIAN_POINT ( 'NONE',  ( -33.39910372087116031, 76.99404724422815605, -3.489146652177067764 ) ) ;
#18599 = EDGE_CURVE ( 'NONE', #19292, #3901, #1659, .T. ) ;
#18600 = DIRECTION ( 'NONE',  ( -0.5000000000000049960, 0.8660254037844357100, -0.000000000000000000 ) ) ;
#18601 = FACE_OUTER_BOUND ( 'NONE', #15227, .T. ) ;
#18602 = ORIENTED_EDGE ( 'NONE', *, *, #11618, .T. ) ;
#18603 = EDGE_CURVE ( 'NONE', #18175, #4518, #10323, .T. ) ;
#18604 = CARTESIAN_POINT ( 'NONE',  ( 82.86035624684615186, 61.08028851158093175, -25.16487698176234389 ) ) ;
#18605 = CARTESIAN_POINT ( 'NONE',  ( 217.4948448325154970, 10.21421812206089541, -7.132002368301439077 ) ) ;
#18606 = ORIENTED_EDGE ( 'NONE', *, *, #12280, .T. ) ;
#18607 = CARTESIAN_POINT ( 'NONE',  ( 202.4235407509943911, 25.03004461941911529, -15.49999243318709574 ) ) ;
#18608 = CARTESIAN_POINT ( 'NONE',  ( -3.350687231550970147, 64.83636698465690529, 2.499114823701145571 ) ) ;
#18609 = CIRCLE ( 'NONE', #1380, 12.50000000000000000 ) ;
#18610 = EDGE_CURVE ( 'NONE', #6420, #19414, #2447, .T. ) ;
#18611 = DIRECTION ( 'NONE',  ( 0.000000000000000000, 0.000000000000000000, -1.000000000000000000 ) ) ;
#18612 = DIRECTION ( 'NONE',  ( 0.8660254037844372643, 0.5000000000000026645, 0.000000000000000000 ) ) ;
#18613 = CARTESIAN_POINT ( 'NONE',  ( 79.17199999999999704, 0.000000000000000000, 0.000000000000000000 ) ) ;
#18614 = VECTOR ( 'NONE', #14200, 1000.000000000000000 ) ;
#18615 = EDGE_CURVE ( 'NONE', #9958, #15512, #8900, .T. ) ;
#18616 = EDGE_LOOP ( 'NONE', ( #20598, #16217, #14100, #6655 ) ) ;
#18617 = VERTEX_POINT ( 'NONE', #10798 ) ;
#18618 = DIRECTION ( 'NONE',  ( 0.8660254037844355990, 0.5000000000000054401, 0.000000000000000000 ) ) ;
#18619 = DIRECTION ( 'NONE',  ( -0.5000000000000049960, 0.8660254037844357100, -0.000000000000000000 ) ) ;
#18620 = VECTOR ( 'NONE', #13857, 999.9999999999998863 ) ;
#18621 = ORIENTED_EDGE ( 'NONE', *, *, #7926, .F. ) ;
#18622 = ORIENTED_EDGE ( 'NONE', *, *, #20480, .F. ) ;
#18623 = ORIENTED_EDGE ( 'NONE', *, *, #14693, .T. ) ;
#18624 = CARTESIAN_POINT ( 'NONE',  ( 195.1605391527415350, 3.615661520069893164, -12.56470246848373229 ) ) ;
#18625 = DIRECTION ( 'NONE',  ( 0.8660254037844352659, 0.5000000000000056621, 0.000000000000000000 ) ) ;
#18626 = CARTESIAN_POINT ( 'NONE',  ( 227.9553588074475954, 39.88513931160571957, -14.00000000000005507 ) ) ;
#18627 = EDGE_CURVE ( 'NONE', #1138, #6371, #20346, .T. ) ;
#18628 = LINE ( 'NONE', #14944, #14423 ) ;
#18629 = CARTESIAN_POINT ( 'NONE',  ( -19.90320481066766689, 68.50873499742380091, -3.129598480498279045 ) ) ;
#18630 = VECTOR ( 'NONE', #7236, 1000.000000000000000 ) ;
#18631 = VERTEX_POINT ( 'NONE', #9203 ) ;
#18632 = CIRCLE ( 'NONE', #351, 3.902363844300875240 ) ;
#18633 = DIRECTION ( 'NONE',  ( 1.000000000000000000, 0.000000000000000000, -5.175391130484829193E-17 ) ) ;
#18634 = ADVANCED_FACE ( 'NONE', ( #753 ), #15398, .T. ) ;
#18635 = B_SPLINE_CURVE_WITH_KNOTS ( 'NONE', 3,
 ( #14359, #4783, #14459, #14560 ),
 .UNSPECIFIED., .F., .F.,
 ( 4, 4 ),
 ( 2.008231194425522893E-05, 0.0005860085342398897983 ),
 .UNSPECIFIED. ) ;
#18636 = DIRECTION ( 'NONE',  ( -0.8660254037844355990, -0.5000000000000055511, 0.000000000000000000 ) ) ;
#18637 = CARTESIAN_POINT ( 'NONE',  ( -22.59901147243187580, 50.26217980097501936, -15.30251921331534426 ) ) ;
#18638 = CARTESIAN_POINT ( 'NONE',  ( 4.000000000000000000, -1.759474945355387954, -3.047499999999997211 ) ) ;
#18639 = DIRECTION ( 'NONE',  ( 0.000000000000000000, 0.000000000000000000, -1.000000000000000000 ) ) ;
#18640 = CARTESIAN_POINT ( 'NONE',  ( -27.41141517789169768, 61.16284628816836744, 5.102783302178296232 ) ) ;
#18642 = ORIENTED_EDGE ( 'NONE', *, *, #19437, .F. ) ;
#18641 = VERTEX_POINT ( 'NONE', #18973 ) ;
#18643 = FACE_OUTER_BOUND ( 'NONE', #16362, .T. ) ;
#18644 = CARTESIAN_POINT ( 'NONE',  ( 62.49954260685851892, 78.23754186779291331, -12.52423913820381607 ) ) ;
#18645 = AXIS2_PLACEMENT_3D ( 'NONE', #16153, #19417, #6468 ) ;
#18646 = ORIENTED_EDGE ( 'NONE', *, *, #12149, .F. ) ;
#18647 = ORIENTED_EDGE ( 'NONE', *, *, #10793, .F. ) ;
#18648 = CARTESIAN_POINT ( 'NONE',  ( 5.000000000000004441, -2.342598717236910044, -4.057499999999996554 ) ) ;
#18649 = CARTESIAN_POINT ( 'NONE',  ( -23.72779897500315727, 50.18955727852706872, -14.96816017130344889 ) ) ;
#18650 = CARTESIAN_POINT ( 'NONE',  ( 217.4465006036304260, 9.413486477856961798, -20.57673792763531040 ) ) ;
#18651 = AXIS2_PLACEMENT_3D ( 'NONE', #12500, #14213, #13996 ) ;
#18652 = ORIENTED_EDGE ( 'NONE', *, *, #9017, .T. ) ;
#18653 = EDGE_LOOP ( 'NONE', ( #2338, #20942, #12715, #17513 ) ) ;
#18654 = DIRECTION ( 'NONE',  ( -0.4999999999999995004, 0.8660254037844390407, 0.000000000000000000 ) ) ;
#18655 = AXIS2_PLACEMENT_3D ( 'NONE', #8423, #3077, #13216 ) ;
#18656 = CARTESIAN_POINT ( 'NONE',  ( -11.10102051443364779, 14.09941697557065332, 0.9999999999999991118 ) ) ;
#18657 = CONICAL_SURFACE ( 'NONE', #16962, 10.85470691220533190, 0.8171114040043576665 ) ;
#18658 = DIRECTION ( 'NONE',  ( -0.8645602258681711616, -0.4991540791356392504, 0.05814482891047982605 ) ) ;
#18659 = CONICAL_SURFACE ( 'NONE', #10152, 13.07248899748297433, 0.6693469023067423196 ) ;
#18660 = DIRECTION ( 'NONE',  ( 1.000000000000000000, -0.000000000000000000, -0.000000000000000000 ) ) ;
#18661 = CIRCLE ( 'NONE', #3758, 19.99999999999999645 ) ;
#18662 = CARTESIAN_POINT ( 'NONE',  ( 228.2946991098875174, 38.64442553422156834, -17.59914077799776422 ) ) ;
#18663 = CARTESIAN_POINT ( 'NONE',  ( 10.40000000000000568, 0.000000000000000000, 0.000000000000000000 ) ) ;
#18664 = DIRECTION ( 'NONE',  ( -0.5000000000000049960, 0.8660254037844357100, 0.000000000000000000 ) ) ;
#18665 = APPLICATION_CONTEXT ( 'automotive_design' ) ;
#18666 = AXIS2_PLACEMENT_3D ( 'NONE', #1573, #1784, #8226 ) ;
#18667 = ORIENTED_EDGE ( 'NONE', *, *, #10054, .T. ) ;
#18668 = LINE ( 'NONE', #646, #17894 ) ;
#18669 = PLANE ( 'NONE',  #17405 ) ;
#18670 = CARTESIAN_POINT ( 'NONE',  ( 221.7398910005669563, 32.78200010370005657, -11.55788255683066268 ) ) ;
#18671 = ORIENTED_EDGE ( 'NONE', *, *, #5629, .T. ) ;
#18672 = CARTESIAN_POINT ( 'NONE',  ( 79.10968724374433236, 57.61535156440357497, -1.789850051334469283 ) ) ;
#18673 = CIRCLE ( 'NONE', #10880, 9.999999999999994671 ) ;
#18674 = ORIENTED_EDGE ( 'NONE', *, *, #20819, .T. ) ;
#18675 = ORIENTED_EDGE ( 'NONE', *, *, #7070, .T. ) ;
#18676 = CARTESIAN_POINT ( 'NONE',  ( 225.7363529196993568, 42.74910436041706419, -12.46964089162983313 ) ) ;
#18677 = CARTESIAN_POINT ( 'NONE',  ( 228.5305256799928486, 38.88892106552724215, -17.38313153181864124 ) ) ;
#18678 = CIRCLE ( 'NONE', #11913, 12.50000000000000000 ) ;
#18679 = AXIS2_PLACEMENT_3D ( 'NONE', #10955, #20588, #2901 ) ;
#18680 = B_SPLINE_CURVE_WITH_KNOTS ( 'NONE', 3,
 ( #10158, #16755, #14981, #2025 ),
 .UNSPECIFIED., .F., .F.,
 ( 4, 4 ),
 ( 2.759414894271772668E-07, 0.0006729267335465118505 ),
 .UNSPECIFIED. ) ;
#18681 = ADVANCED_FACE ( 'NONE', ( #10690 ), #15296, .T. ) ;
#18682 = AXIS2_PLACEMENT_3D ( 'NONE', #12879, #15856, #11074 ) ;
#18683 = PLANE ( 'NONE',  #6879 ) ;
#18684 = ORIENTED_EDGE ( 'NONE', *, *, #4752, .F. ) ;
#18685 = CARTESIAN_POINT ( 'NONE',  ( 61.99529059433388767, 216.5773763115390693, -28.99999999999998934 ) ) ;
#18687 = DIRECTION ( 'NONE',  ( 0.8660254037844352659, 0.5000000000000056621, 0.000000000000000000 ) ) ;
#18686 = B_SPLINE_CURVE_WITH_KNOTS ( 'NONE', 3,
 ( #4780, #9744, #16228, #1705 ),
 .UNSPECIFIED., .F., .F.,
 ( 4, 4 ),
 ( 4.749816698113491977E-07, 0.0004525282234496839418 ),
 .UNSPECIFIED. ) ;
#18688 = CARTESIAN_POINT ( 'NONE',  ( 220.5256391327309302, 34.26729766263312627, -17.38313153181864834 ) ) ;
#18689 = DIRECTION ( 'NONE',  ( 0.8660254037844352659, 0.5000000000000056621, 0.000000000000000000 ) ) ;
#18690 = CARTESIAN_POINT ( 'NONE',  ( 217.2475687086994469, 38.43157579942081270, -12.85003623376098503 ) ) ;
#18691 = AXIS2_PLACEMENT_3D ( 'NONE', #10701, #4661, #7629 ) ;
#18692 = AXIS2_PLACEMENT_3D ( 'NONE', #12985, #16369, #14384 ) ;
#18693 = CIRCLE ( 'NONE', #4794, 14.00000000000000178 ) ;
#18694 = PLANE ( 'NONE',  #16014 ) ;
#18695 = PLANE ( 'NONE',  #4331 ) ;
#18696 = VERTEX_POINT ( 'NONE', #15709 ) ;
#18697 = CARTESIAN_POINT ( 'NONE',  ( 85.37797649651368204, 230.0773763115391262, -26.99999999999999289 ) ) ;
#18698 = CARTESIAN_POINT ( 'NONE',  ( -20.89897948556633978, 16.09941697557071905, 0.9999999999999991118 ) ) ;
#18699 = CARTESIAN_POINT ( 'NONE',  ( 208.4761278624580711, 5.007259451653140125, -14.00000000000005507 ) ) ;
#18700 = EDGE_CURVE ( 'NONE', #15334, #18407, #7203, .T. ) ;
#18702 = ORIENTED_EDGE ( 'NONE', *, *, #16233, .T. ) ;
#18701 = ORIENTED_EDGE ( 'NONE', *, *, #19689, .T. ) ;
#18703 = EDGE_LOOP ( 'NONE', ( #11811, #18507, #6686, #20121, #2012 ) ) ;
#18704 = EDGE_CURVE ( 'NONE', #9959, #10895, #2553, .T. ) ;
#18705 = DIRECTION ( 'NONE',  ( -0.5000000000000008882, 0.8660254037844381525, 0.000000000000000000 ) ) ;
#18706 = DIRECTION ( 'NONE',  ( 0.8660254037844361541, 0.5000000000000044409, -5.976026924694052093E-17 ) ) ;
#18707 = VERTEX_POINT ( 'NONE', #1066 ) ;
#18708 = CONICAL_SURFACE ( 'NONE', #8539, 13.07248899748297433, 0.6693469023067423196 ) ;
#18709 = CARTESIAN_POINT ( 'NONE',  ( -15.99999999999999289, 80.00000000000000000, -12.50000000000000000 ) ) ;
#18710 = UNCERTAINTY_MEASURE_WITH_UNIT (LENGTH_MEASURE( 1.000000000000000082E-05 ), #20717, 'distance_accuracy_value', 'NONE');
#18711 = AXIS2_PLACEMENT_3D ( 'NONE', #14360, #12749, #12650 ) ;
#18712 = DIRECTION ( 'NONE',  ( -0.5000000000000049960, 0.8660254037844358210, -0.000000000000000000 ) ) ;
#18713 = DIRECTION ( 'NONE',  ( -0.8660254037844362651, -0.5000000000000043299, 0.000000000000000000 ) ) ;
#18714 = CARTESIAN_POINT ( 'NONE',  ( 32.00490953756718682, 238.5222400402097662, -18.99999999999997513 ) ) ;
#18715 = EDGE_CURVE ( 'NONE', #5971, #5172, #12314, .T. ) ;
#18716 = DIRECTION ( 'NONE',  ( 0.5000000000000054401, -0.8660254037844354880, 0.000000000000000000 ) ) ;
#18717 = ORIENTED_EDGE ( 'NONE', *, *, #14731, .T. ) ;
#18718 = B_SPLINE_CURVE_WITH_KNOTS ( 'NONE', 3,
 ( #4742, #288, #19463, #19275 ),
 .UNSPECIFIED., .F., .F.,
 ( 4, 4 ),
 ( 1.961874588801930082E-06, 0.0005678880968689130728 ),
 .UNSPECIFIED. ) ;
#18719 = DIRECTION ( 'NONE',  ( -0.6946590618905412740, -0.4010615963775223669, 0.5971585917027958379 ) ) ;
#18720 = FACE_OUTER_BOUND ( 'NONE', #3934, .T. ) ;
#18721 = VECTOR ( 'NONE', #2320, 1000.000000000000000 ) ;
#18722 = EDGE_CURVE ( 'NONE', #10584, #6984, #17935, .T. ) ;
#18723 = LINE ( 'NONE', #3871, #19957 ) ;
#18724 = CARTESIAN_POINT ( 'NONE',  ( 26.99999999999999645, 64.25000000000000000, -2.528164662410438357 ) ) ;
#18725 = DIRECTION ( 'NONE',  ( -0.5000000000000045519, 0.8660254037844360431, 0.000000000000000000 ) ) ;
#18726 = VERTEX_POINT ( 'NONE', #3269 ) ;
#18727 = ORIENTED_EDGE ( 'NONE', *, *, #16127, .T. ) ;
#18728 = DIRECTION ( 'NONE',  ( -0.8660254037844360431, -0.5000000000000044409, 0.000000000000000000 ) ) ;
#18729 = EDGE_CURVE ( 'NONE', #13568, #16059, #2866, .T. ) ;
#18730 = ORIENTED_EDGE ( 'NONE', *, *, #19229, .F. ) ;
#18731 = ORIENTED_EDGE ( 'NONE', *, *, #702, .T. ) ;
#18732 = CARTESIAN_POINT ( 'NONE',  ( 226.2417130873235465, 42.85326076503381643, -12.98880265512658561 ) ) ;
#18733 = CARTESIAN_POINT ( 'NONE',  ( 79.44879617809482397, 49.74114623467382046, -10.15578855070954312 ) ) ;
#18734 = CARTESIAN_POINT ( 'NONE',  ( 208.0983737146324870, 5.661548828456886895, -14.00000000000005507 ) ) ;
#18735 = CARTESIAN_POINT ( 'NONE',  ( 205.8264633344831225, 9.596613037118636669, -14.00000000000005507 ) ) ;
#18736 = CARTESIAN_POINT ( 'NONE',  ( -16.35862578389054889, 71.60341624250784776, -4.990290896351837091 ) ) ;
#18737 = AXIS2_PLACEMENT_3D ( 'NONE', #19311, #14361, #3103 ) ;
#18738 = EDGE_CURVE ( 'NONE', #10851, #2949, #9301, .T. ) ;
#18739 = EDGE_LOOP ( 'NONE', ( #16895, #16380, #18140 ) ) ;
#18740 = ORIENTED_EDGE ( 'NONE', *, *, #19591, .F. ) ;
#18741 = EDGE_CURVE ( 'NONE', #18916, #8377, #741, .T. ) ;
#18742 = CARTESIAN_POINT ( 'NONE',  ( 209.8909370991932235, 2.556737970610013733, -14.00000000000005507 ) ) ;
#18743 = CARTESIAN_POINT ( 'NONE',  ( -30.11049765362162134, 50.08318726096587170, -10.89667398352873029 ) ) ;
#18744 = CARTESIAN_POINT ( 'NONE',  ( 227.9553588074475670, 39.88513931160575510, -14.00000000000005507 ) ) ;
#18745 = EDGE_CURVE ( 'NONE', #2559, #15512, #8033, .T. ) ;
#18746 = CARTESIAN_POINT ( 'NONE',  ( 5.000000000000000000, -3.513898075855355074, 2.028750000000002274 ) ) ;
#18747 = CARTESIAN_POINT ( 'NONE',  ( -35.00000000000000000, 65.74999999999997158, 2.481238266578629226 ) ) ;
#18749 = ORIENTED_EDGE ( 'NONE', *, *, #7656, .F. ) ;
#18748 = ORIENTED_EDGE ( 'NONE', *, *, #18479, .F. ) ;
#18750 = CONICAL_SURFACE ( 'NONE', #9930, 4.172000000000029907, 0.7853981633974425058 ) ;
#18751 = CARTESIAN_POINT ( 'NONE',  ( 220.2180084519553134, 35.41797800104779270, -14.00000000000005507 ) ) ;
#18752 = CARTESIAN_POINT ( 'NONE',  ( 208.5840039954387066, 11.71972914181512060, -2.522505859538486828 ) ) ;
#18753 = DIRECTION ( 'NONE',  ( 0.000000000000000000, 0.000000000000000000, -1.000000000000000000 ) ) ;
#18754 = EDGE_LOOP ( 'NONE', ( #9045, #10272, #13364, #20575 ) ) ;
#18755 = ORIENTED_EDGE ( 'NONE', *, *, #7537, .T. ) ;
#18756 = ORIENTED_EDGE ( 'NONE', *, *, #2740, .T. ) ;
#18757 = CARTESIAN_POINT ( 'NONE',  ( 22.00490953756706958, 255.8427481158984165, -28.99999999999997513 ) ) ;
#18758 = DIRECTION ( 'NONE',  ( -0.05035489893517486326, -0.02907241445524025303, -0.9983081582712680646 ) ) ;
#18759 = CARTESIAN_POINT ( 'NONE',  ( 1.492765116366511435, 53.68125995765908698, -2.649088797068363199 ) ) ;
#18760 = FACE_OUTER_BOUND ( 'NONE', #3026, .T. ) ;
#18761 = EDGE_CURVE ( 'NONE', #2046, #2925, #13133, .T. ) ;
#18762 = ORIENTED_EDGE ( 'NONE', *, *, #17202, .T. ) ;
#18763 = ORIENTED_EDGE ( 'NONE', *, *, #12543, .F. ) ;
#18764 = CARTESIAN_POINT ( 'NONE',  ( 215.3457899893760725, 15.62364810561754958, -18.11117897393244647 ) ) ;
#18765 = B_SPLINE_CURVE_WITH_KNOTS ( 'NONE', 3,
 ( #16525, #5266, #17804, #12940 ),
 .UNSPECIFIED., .F., .F.,
 ( 4, 4 ),
 ( 3.944405719633618568E-05, 0.0006053702794809485152 ),
 .UNSPECIFIED. ) ;
#18766 = EDGE_CURVE ( 'NONE', #9495, #16112, #17922, .T. ) ;
#18767 = LINE ( 'NONE', #7200, #7709 ) ;
#18768 = DIRECTION ( 'NONE',  ( 0.000000000000000000, -1.000000000000000000, 0.000000000000000000 ) ) ;
#18769 = EDGE_CURVE ( 'NONE', #9257, #16672, #1277, .T. ) ;
#18770 = CARTESIAN_POINT ( 'NONE',  ( 226.0729998088514208, 43.14548073525869398, -15.02729838650890493 ) ) ;
#18771 = DIRECTION ( 'NONE',  ( -0.8660254037844360431, -0.5000000000000045519, -0.000000000000000000 ) ) ;
#18772 = CARTESIAN_POINT ( 'NONE',  ( -27.55795892725420160, 70.83821676753269969, 4.766221741044114779 ) ) ;
#18773 = CARTESIAN_POINT ( 'NONE',  ( 213.8661528393178060, 8.119191822981960627, -3.188775577416895324 ) ) ;
#18774 = VERTEX_POINT ( 'NONE', #19385 ) ;
#18775 = CARTESIAN_POINT ( 'NONE',  ( -28.94270596280446739, 74.04855861174519305, -0.5148205403795984569 ) ) ;
#18776 = DIRECTION ( 'NONE',  ( -0.8660254037844360431, -0.5000000000000045519, 0.000000000000000000 ) ) ;
#18777 = CARTESIAN_POINT ( 'NONE',  ( 49.86389338619021316, 127.5895726428436205, -12.50000000000000000 ) ) ;
#18778 = ORIENTED_EDGE ( 'NONE', *, *, #13219, .F. ) ;
#18779 = CARTESIAN_POINT ( 'NONE',  ( 74.42497496061868389, 69.15581319408583738, -0.1672178410544389870 ) ) ;
#18780 = EDGE_LOOP ( 'NONE', ( #12306, #8665, #19562, #11326 ) ) ;
#18781 = VERTEX_POINT ( 'NONE', #7724 ) ;
#18782 = DIRECTION ( 'NONE',  ( -0.5000000000000054401, 0.8660254037844354880, -0.000000000000000000 ) ) ;
#18783 = AXIS2_PLACEMENT_3D ( 'NONE', #10634, #2914, #19030 ) ;
#18784 = DIRECTION ( 'NONE',  ( 0.8660254037844355990, 0.5000000000000054401, 0.000000000000000000 ) ) ;
#18785 = DIRECTION ( 'NONE',  ( 0.9990858356752083669, 0.04274918657905462521, 0.000000000000000000 ) ) ;
#18786 = CARTESIAN_POINT ( 'NONE',  ( 214.9079348888216998, 19.49485026284914113, -11.01983352639526892 ) ) ;
#18787 = EDGE_LOOP ( 'NONE', ( #4536, #5515 ) ) ;
#18788 = CYLINDRICAL_SURFACE ( 'NONE', #12807, 9.999999999999998224 ) ;
#18789 = DIRECTION ( 'NONE',  ( 0.3430151393149032946, 0.1980398830195792548, -0.9182161068802751069 ) ) ;
#18790 = FACE_BOUND ( 'NONE', #18787, .T. ) ;
#18791 = CARTESIAN_POINT ( 'NONE',  ( 197.7356731787758690, -1.966565041833207017, -17.08769543353810860 ) ) ;
#18792 = CARTESIAN_POINT ( 'NONE',  ( 202.6529885701316971, 8.118445885262769224, -2.363289276295887920 ) ) ;
#18793 = CARTESIAN_POINT ( 'NONE',  ( 216.3403026830736735, 15.84380369567995039, -15.42323214253238284 ) ) ;
#18794 = DIRECTION ( 'NONE',  ( 0.000000000000000000, -0.9359693004502238622, -0.3520816220916943573 ) ) ;
#18795 = EDGE_CURVE ( 'NONE', #4228, #12427, #1684, .T. ) ;
#18796 = VECTOR ( 'NONE', #19669, 1000.000000000000114 ) ;
#18797 = CARTESIAN_POINT ( 'NONE',  ( 69.99529059433403688, 202.7209698509880411, 11.00000000000001066 ) ) ;
#18798 = ORIENTED_EDGE ( 'NONE', *, *, #8425, .F. ) ;
#18799 = CARTESIAN_POINT ( 'NONE',  ( 228.6455928494450234, 37.71015299068947257, -17.20332536629375753 ) ) ;
#18800 = CARTESIAN_POINT ( 'NONE',  ( 208.0983737146324870, 5.661548828456886895, -14.00000000000005507 ) ) ;
#18801 = DIRECTION ( 'NONE',  ( -0.8660254037844360431, -0.5000000000000043299, 0.000000000000000000 ) ) ;
#18802 = B_SPLINE_CURVE_WITH_KNOTS ( 'NONE', 3,
 ( #16849, #8787, #3802, #18650 ),
 .UNSPECIFIED., .F., .F.,
 ( 4, 4 ),
 ( 6.440264277512764414E-07, 0.0008546297644107766264 ),
 .UNSPECIFIED. ) ;
#18804 = ORIENTED_EDGE ( 'NONE', *, *, #7965, .F. ) ;
#18803 = ORIENTED_EDGE ( 'NONE', *, *, #20309, .F. ) ;
#18805 = ORIENTED_EDGE ( 'NONE', *, *, #18453, .T. ) ;
#18806 = CARTESIAN_POINT ( 'NONE',  ( -13.48852428594715747, 10.76355435230335011, 12.24827897062957227 ) ) ;
#18807 = DIRECTION ( 'NONE',  ( 6.608470384673549052E-16, -1.000000000000000000, 0.000000000000000000 ) ) ;
#18808 = ORIENTED_EDGE ( 'NONE', *, *, #1507, .F. ) ;
#18809 = EDGE_CURVE ( 'NONE', #15099, #12098, #16116, .T. ) ;
#18810 = DIRECTION ( 'NONE',  ( 0.000000000000000000, 1.000000000000000000, 0.000000000000000000 ) ) ;
#18811 = AXIS2_PLACEMENT_3D ( 'NONE', #16873, #13701, #8812 ) ;
#18812 = DIRECTION ( 'NONE',  ( -0.5000000000000047740, 0.8660254037844358210, 0.000000000000000000 ) ) ;
#18813 = VECTOR ( 'NONE', #9000, 1000.000000000000000 ) ;
#18814 =( NAMED_UNIT ( * ) SI_UNIT ( $, .STERADIAN. ) SOLID_ANGLE_UNIT ( ) );
#18815 = DIRECTION ( 'NONE',  ( 0.000000000000000000, -0.8174753238307638226, 0.5759636229205693514 ) ) ;
#18816 = DIRECTION ( 'NONE',  ( 1.000000000000000000, 0.000000000000000000, 0.000000000000000000 ) ) ;
#18817 = DIRECTION ( 'NONE',  ( 1.000000000000000000, 0.000000000000000000, 0.000000000000000000 ) ) ;
#18818 = EDGE_CURVE ( 'NONE', #16059, #3334, #4554, .T. ) ;
#18819 = EDGE_LOOP ( 'NONE', ( #10734, #4090, #12245 ) ) ;
#18820 = ADVANCED_FACE ( 'NONE', ( #6534 ), #9516, .F. ) ;
#18821 = CARTESIAN_POINT ( 'NONE',  ( 225.6000782901530215, 42.98513894257393986, -14.55761806292083982 ) ) ;
#18822 = FACE_OUTER_BOUND ( 'NONE', #7683, .T. ) ;
#18823 = CARTESIAN_POINT ( 'NONE',  ( -14.99999999999999645, -10.00000000000000000, -30.00000000000000000 ) ) ;
#18824 = CYLINDRICAL_SURFACE ( 'NONE', #1708, 5.000000000000000000 ) ;
#18825 = DIRECTION ( 'NONE',  ( -1.000000000000000000, 0.000000000000000000, 3.517351572405780687E-16 ) ) ;
#18826 = AXIS2_PLACEMENT_3D ( 'NONE', #7843, #5934, #14344 ) ;
#18828 = VERTEX_POINT ( 'NONE', #7826 ) ;
#18827 = VERTEX_POINT ( 'NONE', #13035 ) ;
#18829 = EDGE_LOOP ( 'NONE', ( #20556, #16923, #6557, #9449, #9785, #10692 ) ) ;
#18830 = AXIS2_PLACEMENT_3D ( 'NONE', #9183, #16941, #18949 ) ;
#18831 = DIRECTION ( 'NONE',  ( -1.000000000000000000, -0.000000000000000000, -0.000000000000000000 ) ) ;
#18832 = ORIENTED_EDGE ( 'NONE', *, *, #16163, .T. ) ;
#18833 = ORIENTED_EDGE ( 'NONE', *, *, #104, .F. ) ;
#18834 = VERTEX_POINT ( 'NONE', #7925 ) ;
#18835 = DIRECTION ( 'NONE',  ( 0.000000000000000000, 0.000000000000000000, -1.000000000000000000 ) ) ;
#18836 = CARTESIAN_POINT ( 'NONE',  ( 79.71277097872595618, 50.46579360009113202, -7.932047079679189316 ) ) ;
#18837 = CARTESIAN_POINT ( 'NONE',  ( 202.8297164780629487, 0.8660905863451863196, -14.00000000000005507 ) ) ;
#18838 = DIRECTION ( 'NONE',  ( -0.5000000000000054401, 0.8660254037844354880, -0.000000000000000000 ) ) ;
#18839 = TOROIDAL_SURFACE ( 'NONE', #1244, 6.960520131757804485, 1.000000000000000000 ) ;
#18840 = ORIENTED_EDGE ( 'NONE', *, *, #14641, .T. ) ;
#18841 = AXIS2_PLACEMENT_3D ( 'NONE', #18937, #20512, #20618 ) ;
#18842 = CIRCLE ( 'NONE', #4242, 5.000000000000035527 ) ;
#18843 = PLANE ( 'NONE',  #16910 ) ;
#18844 = EDGE_CURVE ( 'NONE', #9959, #112, #6431, .T. ) ;
#18845 = ADVANCED_FACE ( 'NONE', ( #12718 ), #4859, .F. ) ;
#18846 = CARTESIAN_POINT ( 'NONE',  ( -18.93604315306787100, 49.50911328882459372, -12.15750417611710787 ) ) ;
#18847 = DIRECTION ( 'NONE',  ( -0.5000000000000046629, 0.8660254037844359321, 0.000000000000000000 ) ) ;
#18848 = CARTESIAN_POINT ( 'NONE',  ( 225.9071529074726925, 43.43273599472491497, -15.14518239232895347 ) ) ;
#18849 = FACE_OUTER_BOUND ( 'NONE', #7487, .T. ) ;
#18851 = ORIENTED_EDGE ( 'NONE', *, *, #17260, .F. ) ;
#18850 = ORIENTED_EDGE ( 'NONE', *, *, #8879, .T. ) ;
#18852 = EDGE_LOOP ( 'NONE', ( #6440, #13386, #12498, #17504 ) ) ;
#18853 = CARTESIAN_POINT ( 'NONE',  ( 219.9346875340479244, 35.49677405717110190, -17.67703110843606851 ) ) ;
#18854 = CARTESIAN_POINT ( 'NONE',  ( 215.9829844511909300, 15.46048323788008361, -18.25196083293883120 ) ) ;
#18855 = CARTESIAN_POINT ( 'NONE',  ( -3.510843195177423492, 80.00000000000000000, 0.5205403966592451193 ) ) ;
#18856 = VERTEX_POINT ( 'NONE', #20856 ) ;
#18857 = ORIENTED_EDGE ( 'NONE', *, *, #11046, .F. ) ;
#18858 = EDGE_CURVE ( 'NONE', #19734, #10275, #6329, .T. ) ;
#18859 = EDGE_LOOP ( 'NONE', ( #10646, #15563, #17746, #10963 ) ) ;
#18860 = AXIS2_PLACEMENT_3D ( 'NONE', #1551, #9987, #3542 ) ;
#18861 = DIRECTION ( 'NONE',  ( 0.8660254037844355990, 0.5000000000000054401, 0.000000000000000000 ) ) ;
#18862 = CARTESIAN_POINT ( 'NONE',  ( 196.1782232529825762, 4.026199028858075124, -19.61257667712936126 ) ) ;
#18863 = CARTESIAN_POINT ( 'NONE',  ( -33.35732806943984485, 52.10193024710888210, -4.832466544100828543 ) ) ;
#18864 = CARTESIAN_POINT ( 'NONE',  ( -26.77079800181776648, 9.903286195278038662, -6.378645726547156336 ) ) ;
#18865 = ORIENTED_EDGE ( 'NONE', *, *, #9775, .T. ) ;
#18866 = ORIENTED_EDGE ( 'NONE', *, *, #7047, .F. ) ;
#18867 = DIRECTION ( 'NONE',  ( 0.8660254037844368202, 0.5000000000000031086, 1.665334536937734564E-16 ) ) ;
#18868 = ADVANCED_FACE ( 'NONE', ( #19284 ), #8022, .F. ) ;
#18869 = LINE ( 'NONE', #12084, #13139 ) ;
#18870 = CARTESIAN_POINT ( 'NONE',  ( 221.5988438203954729, 32.40845261667698907, -12.62147488791611849 ) ) ;
#18871 = CARTESIAN_POINT ( 'NONE',  ( -11.03378583276534108, 15.76606607271690841, 11.47134211267085391 ) ) ;
#18872 = EDGE_CURVE ( 'NONE', #1818, #17716, #17799, .T. ) ;
#18873 = CIRCLE ( 'NONE', #11419, 6.500000000000000888 ) ;
#18874 = DIRECTION ( 'NONE',  ( 0.8660254037844377084, 0.5000000000000017764, -1.040834085586084380E-16 ) ) ;
#18875 = DIRECTION ( 'NONE',  ( 0.000000000000000000, -6.938893903907177533E-18, -1.000000000000000000 ) ) ;
#18876 = DIRECTION ( 'NONE',  ( -0.8660254037844360431, -0.5000000000000044409, 5.976026924694052093E-17 ) ) ;
#18877 = VERTEX_POINT ( 'NONE', #18210 ) ;
#18878 = CIRCLE ( 'NONE', #5990, 5.000000000000036415 ) ;
#18879 = FACE_OUTER_BOUND ( 'NONE', #7558, .T. ) ;
#18880 = CARTESIAN_POINT ( 'NONE',  ( 228.9655759139732538, 38.13539195642837143, -16.94731950718130520 ) ) ;
#18881 = LINE ( 'NONE', #4353, #17309 ) ;
#18882 = ORIENTED_EDGE ( 'NONE', *, *, #11627, .F. ) ;
#18883 = CARTESIAN_POINT ( 'NONE',  ( 82.33324130691016762, 62.82700397177379870, 0.3205479543778964602 ) ) ;
#18884 = EDGE_CURVE ( 'NONE', #12839, #14228, #299, .T. ) ;
#18885 = ORIENTED_EDGE ( 'NONE', *, *, #8734, .F. ) ;
#18886 = ADVANCED_FACE ( 'NONE', ( #10024 ), #14848, .T. ) ;
#18887 = VERTEX_POINT ( 'NONE', #6743 ) ;
#18888 = CARTESIAN_POINT ( 'NONE',  ( -4.574195094169405174, 69.03990363093106453, 5.071150534606958971 ) ) ;
#18889 = DIRECTION ( 'NONE',  ( 0.4999999999999995004, -0.8660254037844390407, 0.000000000000000000 ) ) ;
#18890 = AXIS2_PLACEMENT_3D ( 'NONE', #17330, #2814, #18713 ) ;
#18891 = PRODUCT_CONTEXT ( 'NONE', #19729, 'mechanical' ) ;
#18892 = EDGE_CURVE ( 'NONE', #2720, #9060, #14546, .T. ) ;
#18893 = CIRCLE ( 'NONE', #7370, 3.902363844300875240 ) ;
#18894 = DIRECTION ( 'NONE',  ( 1.153604387573318063E-16, -8.028960261725416899E-17, 1.000000000000000000 ) ) ;
#18895 = EDGE_LOOP ( 'NONE', ( #14315, #15819, #3489, #20622 ) ) ;
#18896 = CARTESIAN_POINT ( 'NONE',  ( 31.85427444295656940, 188.7831476774788655, 11.00000000000001421 ) ) ;
#18897 = DIRECTION ( 'NONE',  ( 0.8660254037844370423, 0.5000000000000026645, -0.000000000000000000 ) ) ;
#18898 = DIRECTION ( 'NONE',  ( -0.5000000000000047740, 0.8660254037844358210, 0.000000000000000000 ) ) ;
#18899 = FACE_OUTER_BOUND ( 'NONE', #3986, .T. ) ;
#18900 = ORIENTED_EDGE ( 'NONE', *, *, #7939, .F. ) ;
#18901 = DIRECTION ( 'NONE',  ( -0.5000000000000045519, 0.8660254037844360431, -2.168404344971014538E-16 ) ) ;
#18902 = EDGE_CURVE ( 'NONE', #6444, #16315, #6013, .T. ) ;
#18903 = CARTESIAN_POINT ( 'NONE',  ( 27.00000000000002487, 65.74999999999997158, 2.481238266578629226 ) ) ;
#18904 = FACE_OUTER_BOUND ( 'NONE', #14252, .T. ) ;
#18905 = VECTOR ( 'NONE', #7386, 1000.000000000000114 ) ;
#18906 = DIRECTION ( 'NONE',  ( -0.4953429730181675983, 0.8579591964396817705, 0.1361666490962400167 ) ) ;
#18907 = ORIENTED_EDGE ( 'NONE', *, *, #2554, .T. ) ;
#18908 = FACE_OUTER_BOUND ( 'NONE', #7121, .T. ) ;
#18909 = DIRECTION ( 'NONE',  ( -1.000000000000000000, -0.000000000000000000, -0.000000000000000000 ) ) ;
#18910 = DIRECTION ( 'NONE',  ( -0.5000000000000054401, 0.8660254037844354880, -0.000000000000000000 ) ) ;
#18911 = CARTESIAN_POINT ( 'NONE',  ( -28.50080181521929745, 80.00000000000000000, 0.2411454413934158159 ) ) ;
#18913 = ORIENTED_EDGE ( 'NONE', *, *, #5508, .T. ) ;
#18912 = ORIENTED_EDGE ( 'NONE', *, *, #19357, .T. ) ;
#18914 = CARTESIAN_POINT ( 'NONE',  ( 221.5988438203954729, 32.40845261667698907, -12.62147488791611849 ) ) ;
#18915 = DIRECTION ( 'NONE',  ( -1.000000000000000000, 0.000000000000000000, 0.000000000000000000 ) ) ;
#18916 = VERTEX_POINT ( 'NONE', #1895 ) ;
#18917 = DIRECTION ( 'NONE',  ( 0.5000000000000051070, -0.8660254037844359321, 0.000000000000000000 ) ) ;
#18918 = AXIS2_PLACEMENT_3D ( 'NONE', #10499, #18897, #1299 ) ;
#18919 = CARTESIAN_POINT ( 'NONE',  ( 218.1839418517603235, 38.32323632922017254, -14.53509620734043217 ) ) ;
#18920 = CARTESIAN_POINT ( 'NONE',  ( 206.2654030616020293, 10.38108426852119770, -13.50586075465474423 ) ) ;
#18921 = CARTESIAN_POINT ( 'NONE',  ( 201.5089327760127844, 7.457924964560246117, -2.844109184787520839 ) ) ;
#18922 = ORIENTED_EDGE ( 'NONE', *, *, #18965, .T. ) ;
#18923 = CARTESIAN_POINT ( 'NONE',  ( 81.06711713768373784, 65.00000000000000000, -25.50000000000000000 ) ) ;
#18924 = CARTESIAN_POINT ( 'NONE',  ( 205.0662616026534693, 10.91332106064940888, -14.00000000000005507 ) ) ;
#18925 = CARTESIAN_POINT ( 'NONE',  ( -11.10102051443364779, 16.09941697557071905, 0.9999999999999997780 ) ) ;
#18926 = CARTESIAN_POINT ( 'NONE',  ( 218.0578026990161504, 37.02820936217296577, -16.57782486433068314 ) ) ;
#18927 = VECTOR ( 'NONE', #6881, 1000.000000000000114 ) ;
#18929 = ORIENTED_EDGE ( 'NONE', *, *, #20138, .T. ) ;
#18928 = ORIENTED_EDGE ( 'NONE', *, *, #12744, .T. ) ;
#18930 = VERTEX_POINT ( 'NONE', #3675 ) ;
#18931 = PLANE ( 'NONE',  #15983 ) ;
#18932 = PRODUCT_DEFINITION_FORMATION_WITH_SPECIFIED_SOURCE ( 'ANY', '', #10402, .NOT_KNOWN. ) ;
#18933 = ORIENTED_EDGE ( 'NONE', *, *, #15917, .T. ) ;
#18934 = EDGE_LOOP ( 'NONE', ( #4130, #20292 ) ) ;
#18935 = LINE ( 'NONE', #15770, #2127 ) ;
#18936 = DIRECTION ( 'NONE',  ( 0.000000000000000000, 0.000000000000000000, -1.000000000000000000 ) ) ;
#18937 = CARTESIAN_POINT ( 'NONE',  ( 211.6737232845934500, 17.62757732253168541, -21.59012016402730083 ) ) ;
#18938 = CARTESIAN_POINT ( 'NONE',  ( 226.3952283206526772, 41.60789869010848463, -10.82724490084729929 ) ) ;
#18939 = EDGE_CURVE ( 'NONE', #18162, #4848, #11534, .T. ) ;
#18940 = DIRECTION ( 'NONE',  ( 0.000000000000000000, 6.938893903907178303E-18, 1.000000000000000000 ) ) ;
#18941 = ORIENTED_EDGE ( 'NONE', *, *, #14306, .F. ) ;
#18942 = AXIS2_PLACEMENT_3D ( 'NONE', #14193, #17566, #17460 ) ;
#18943 = CARTESIAN_POINT ( 'NONE',  ( 205.5965122587965084, 9.994899983462953941, -14.00000000000005507 ) ) ;
#18944 = CARTESIAN_POINT ( 'NONE',  ( -25.65654271851453316, 45.04382983066486190, -7.944781169143150912 ) ) ;
#18945 = PLANE ( 'NONE',  #18398 ) ;
#18946 = CIRCLE ( 'NONE', #5731, 11.94520687646042667 ) ;
#18947 = DIRECTION ( 'NONE',  ( 1.000000000000000000, -0.000000000000000000, -0.000000000000000000 ) ) ;
#18948 = ADVANCED_FACE ( 'NONE', ( #10129 ), #19578, .T. ) ;
#18949 = DIRECTION ( 'NONE',  ( -0.8660254037844355990, -0.5000000000000054401, -1.599177586275613688E-14 ) ) ;
#18951 = ORIENTED_EDGE ( 'NONE', *, *, #12744, .F. ) ;
#18950 = VERTEX_POINT ( 'NONE', #6860 ) ;
#18952 = ORIENTED_EDGE ( 'NONE', *, *, #20514, .T. ) ;
#18953 = CARTESIAN_POINT ( 'NONE',  ( 218.5801281010350863, 37.63702161621608866, -16.29291827778579815 ) ) ;
#18954 = LINE ( 'NONE', #9391, #16612 ) ;
#18955 = CARTESIAN_POINT ( 'NONE',  ( 0.9782604970530670574, 77.74400922168841532, -4.586390192071695182 ) ) ;
#18956 = ORIENTED_EDGE ( 'NONE', *, *, #5232, .F. ) ;
#18957 = ORIENTED_EDGE ( 'NONE', *, *, #19792, .F. ) ;
#18958 = ORIENTED_EDGE ( 'NONE', *, *, #13206, .T. ) ;
#18959 = CARTESIAN_POINT ( 'NONE',  ( 195.4216187824591202, 18.83910615367374675, -14.00000000000005507 ) ) ;
#18960 = DIRECTION ( 'NONE',  ( 1.000000000000000000, 0.000000000000000000, 0.000000000000000000 ) ) ;
#18961 = CARTESIAN_POINT ( 'NONE',  ( -33.32166605174446516, 55.08543698672535527, -1.237103341644910648 ) ) ;
#18962 = VECTOR ( 'NONE', #11077, 1000.000000000000227 ) ;
#18963 = CARTESIAN_POINT ( 'NONE',  ( -26.41437051192821883, 9.999999999999996447, 6.947505984095691645 ) ) ;
#18964 = VERTEX_POINT ( 'NONE', #10238 ) ;
#18965 = EDGE_CURVE ( 'NONE', #1345, #13223, #15164, .T. ) ;
#18966 = VECTOR ( 'NONE', #3983, 1000.000000000000114 ) ;
#18967 = VERTEX_POINT ( 'NONE', #2108 ) ;
#18968 = EDGE_CURVE ( 'NONE', #12002, #4596, #18594, .T. ) ;
#18969 = LINE ( 'NONE', #10905, #14486 ) ;
#18970 = ORIENTED_EDGE ( 'NONE', *, *, #3087, .F. ) ;
#18971 = AXIS2_PLACEMENT_3D ( 'NONE', #8702, #972, #7108 ) ;
#18972 = CARTESIAN_POINT ( 'NONE',  ( 47.11964624731579221, 270.3427481158987007, -13.99999999999998757 ) ) ;
#18973 = CARTESIAN_POINT ( 'NONE',  ( 195.0692117681097955, 18.22871929987706352, -14.00000000000005507 ) ) ;
#18974 = CIRCLE ( 'NONE', #689, 11.98469917212512215 ) ;
#18975 = EDGE_CURVE ( 'NONE', #18220, #15844, #14382, .T. ) ;
#18976 = LINE ( 'NONE', #10916, #7495 ) ;
#18977 = LINE ( 'NONE', #1176, #18206 ) ;
#18978 = LINE ( 'NONE', #15301, #5168 ) ;
#18979 = VECTOR ( 'NONE', #14260, 1000.000000000000114 ) ;
#18980 = DIRECTION ( 'NONE',  ( -0.8660254037844355990, -0.5000000000000054401, 3.379131769260644202E-14 ) ) ;
#18981 = VECTOR ( 'NONE', #10297, 1000.000000000000000 ) ;
#18982 = DIRECTION ( 'NONE',  ( 0.000000000000000000, -0.000000000000000000, -1.000000000000000000 ) ) ;
#18983 = DIRECTION ( 'NONE',  ( 0.8660254037844361541, 0.5000000000000044409, 0.000000000000000000 ) ) ;
#18984 = B_SPLINE_CURVE_WITH_KNOTS ( 'NONE', 3,
 ( #9177, #15684, #20523, #5994 ),
 .UNSPECIFIED., .F., .F.,
 ( 4, 4 ),
 ( 3.205833042637825210E-07, 0.0004523738250841245040 ),
 .UNSPECIFIED. ) ;
#18985 = ORIENTED_EDGE ( 'NONE', *, *, #16467, .T. ) ;
#18987 = ADVANCED_FACE ( 'NONE', ( #517 ), #6962, .F. ) ;
#18986 = CARTESIAN_POINT ( 'NONE',  ( 70.88304643526481641, 70.79367311254448225, -0.8473711193443549394 ) ) ;
#18988 = AXIS2_PLACEMENT_3D ( 'NONE', #17090, #18782, #3935 ) ;
#18989 = ORIENTED_EDGE ( 'NONE', *, *, #6610, .F. ) ;
#18990 = EDGE_LOOP ( 'NONE', ( #13330, #7750, #16080, #12057 ) ) ;
#18991 = CARTESIAN_POINT ( 'NONE',  ( -3.056599057715243095, 73.00589460461357305, 0.1996236911402666236 ) ) ;
#18992 = EDGE_CURVE ( 'NONE', #7993, #3963, #13087, .T. ) ;
#18993 = VECTOR ( 'NONE', #1707, 1000.000000000000227 ) ;
#18994 = ITEM_DEFINED_TRANSFORMATION ( 'NONE', 'NONE', #7039,  #18233 ) ;
#18995 = VECTOR ( 'NONE', #10064, 1000.000000000000114 ) ;
#18996 = CIRCLE ( 'NONE', #11883, 12.47473710546057823 ) ;
#18997 = LINE ( 'NONE', #8045, #14711 ) ;
#18998 = CARTESIAN_POINT ( 'NONE',  ( 218.4348361543091812, 9.984102274091050333, -18.06789442459602668 ) ) ;
#18999 = CARTESIAN_POINT ( 'NONE',  ( 199.2657312721003393, 25.05322593869168202, -14.00000000000005507 ) ) ;
#19000 = CARTESIAN_POINT ( 'NONE',  ( 221.1115843835763144, 31.73890432929152894, -11.78784277354610133 ) ) ;
#19001 = DIRECTION ( 'NONE',  ( 0.5000000000000051070, -0.8660254037844359321, 0.000000000000000000 ) ) ;
#19002 = AXIS2_PLACEMENT_3D ( 'NONE', #19133, #19240, #5972 ) ;
#19003 = ADVANCED_FACE ( 'NONE', ( #14744, #8344 ), #198, .F. ) ;
#19004 = EDGE_CURVE ( 'NONE', #19163, #3127, #13134, .T. ) ;
#19005 = FACE_OUTER_BOUND ( 'NONE', #7660, .T. ) ;
#19006 = CARTESIAN_POINT ( 'NONE',  ( 64.01452848080103308, 153.0799536996103996, 56.00000000000000711 ) ) ;
#19007 = CIRCLE ( 'NONE', #6806, 11.94520687646042667 ) ;
#19008 = CARTESIAN_POINT ( 'NONE',  ( 219.1969384858217325, 10.68170148414690779, -13.99502662667482866 ) ) ;
#19009 = PLANE ( 'NONE',  #20012 ) ;
#19010 = DIRECTION ( 'NONE',  ( 0.000000000000000000, 0.4999999999999983347, -0.8660254037844395958 ) ) ;
#19011 = ORIENTED_EDGE ( 'NONE', *, *, #3519, .F. ) ;
#19012 = VECTOR ( 'NONE', #11268, 1000.000000000000000 ) ;
#19013 = AXIS2_PLACEMENT_3D ( 'NONE', #17972, #14706, #16382 ) ;
#19015 = ADVANCED_FACE ( 'NONE', ( #16518 ), #8446, .T. ) ;
#19014 = CARTESIAN_POINT ( 'NONE',  ( 93.04593889385130012, 210.2557651598135351, 11.00000000000001066 ) ) ;
#19016 = CYLINDRICAL_SURFACE ( 'NONE', #4063, 11.99999999999999822 ) ;
#19017 = VECTOR ( 'NONE', #17235, 1000.000000000000000 ) ;
#19018 = DIRECTION ( 'NONE',  ( 0.5171545105027588463, 0.2985792958514009166, 0.8021231927550366292 ) ) ;
#19019 = CARTESIAN_POINT ( 'NONE',  ( 203.2336538649942668, 12.75470097114692969, -25.81526893633797570 ) ) ;
#19020 = PLANE ( 'NONE',  #3010 ) ;
#19022 = ORIENTED_EDGE ( 'NONE', *, *, #9891, .F. ) ;
#19021 = ORIENTED_EDGE ( 'NONE', *, *, #814, .F. ) ;
#19023 = ORIENTED_EDGE ( 'NONE', *, *, #17239, .F. ) ;
#19024 = CARTESIAN_POINT ( 'NONE',  ( -12.94451012642581667, 11.12812038848359641, 12.12401870821426719 ) ) ;
#19025 = CARTESIAN_POINT ( 'NONE',  ( -16.00000000000007105, 58.38562172233837089, -4.999999999999997335 ) ) ;
#19026 = EDGE_LOOP ( 'NONE', ( #2541, #657 ) ) ;
#19027 = EDGE_CURVE ( 'NONE', #14420, #17970, #5573, .T. ) ;
#19028 = CARTESIAN_POINT ( 'NONE',  ( 1.500000000000001332, 9.242062880866249359E-16, -8.000000000000000000 ) ) ;
#19029 = DIRECTION ( 'NONE',  ( -0.8660254037844380415, -0.5000000000000014433, -0.000000000000000000 ) ) ;
#19030 = DIRECTION ( 'NONE',  ( 0.8660254037844352659, 0.5000000000000056621, 0.000000000000000000 ) ) ;
#19031 = ADVANCED_FACE ( 'NONE', ( #5889 ), #9072, .T. ) ;
#19032 = VECTOR ( 'NONE', #18874, 999.9999999999998863 ) ;
#19033 = CARTESIAN_POINT ( 'NONE',  ( -31.82323003959540486, 65.74999999999997158, 2.481238266578629226 ) ) ;
#19034 =( NAMED_UNIT ( * ) SI_UNIT ( $, .STERADIAN. ) SOLID_ANGLE_UNIT ( ) );
#19035 = ORIENTED_EDGE ( 'NONE', *, *, #12792, .T. ) ;
#19036 = PLANE ( 'NONE',  #19002 ) ;
#19037 = CARTESIAN_POINT ( 'NONE',  ( 226.1656734413107870, 42.98496529531720256, -14.53826389233644356 ) ) ;
#19038 = DIRECTION ( 'NONE',  ( 0.5000000000000051070, -0.8660254037844359321, 0.000000000000000000 ) ) ;
#19039 = CARTESIAN_POINT ( 'NONE',  ( -29.99999999999999645, 5.000000000000000000, 15.00000000000000000 ) ) ;
#19040 = ORIENTED_EDGE ( 'NONE', *, *, #17554, .T. ) ;
#19041 = VERTEX_POINT ( 'NONE', #20211 ) ;
#19042 = CONICAL_SURFACE ( 'NONE', #8184, 4.509097725792825528, 0.5235987755983015912 ) ;
#19043 = DIRECTION ( 'NONE',  ( 0.000000000000000000, 0.000000000000000000, -1.000000000000000000 ) ) ;
#19044 = CIRCLE ( 'NONE', #4807, 11.98469917212512215 ) ;
#19045=STYLED_ITEM('',(#20974),#10635);
#19046 = ORIENTED_EDGE ( 'NONE', *, *, #11627, .T. ) ;
#19047 = ORIENTED_EDGE ( 'NONE', *, *, #17554, .F. ) ;
#19048 = DIRECTION ( 'NONE',  ( -0.8601696498176565342, -0.4966191788709772847, -0.1160929141252230318 ) ) ;
#19049 = CARTESIAN_POINT ( 'NONE',  ( 79.58732107615884388, 50.12062531598694193, -8.807143433601581251 ) ) ;
#19050 = DIRECTION ( 'NONE',  ( -0.000000000000000000, 1.000000000000000000, -0.000000000000000000 ) ) ;
#19051 = DIRECTION ( 'NONE',  ( 0.5000000000000044409, -0.8660254037844360431, -4.006172263299080068E-16 ) ) ;
#19052 = CARTESIAN_POINT ( 'NONE',  ( 214.8600158830803650, 14.81213703278996618, -20.84195174293595443 ) ) ;
#19053 = ORIENTED_EDGE ( 'NONE', *, *, #13844, .F. ) ;
#19054 = DIRECTION ( 'NONE',  ( 0.3886714912512186371, 0.2243995901002275029, -0.8936326403234182703 ) ) ;
#19055 = CIRCLE ( 'NONE', #16680, 3.619616396367202782 ) ;
#19056 = CARTESIAN_POINT ( 'NONE',  ( -15.99999999999999289, 20.09941697557067997, 12.50000000000000000 ) ) ;
#19057 = CARTESIAN_POINT ( 'NONE',  ( -0.4109910671737397325, 50.38691911710247240, -9.099745271904268407 ) ) ;
#19058 = FACE_OUTER_BOUND ( 'NONE', #15480, .T. ) ;
#19059 = LINE ( 'NONE', #6208, #19294 ) ;
#19060 = CARTESIAN_POINT ( 'NONE',  ( 98.35782272495457335, 199.7505593597859956, 13.41892939600676016 ) ) ;
#19061 = EDGE_CURVE ( 'NONE', #18726, #7315, #17891, .T. ) ;
#19063 = ORIENTED_EDGE ( 'NONE', *, *, #12536, .T. ) ;
#19062 = ORIENTED_EDGE ( 'NONE', *, *, #8567, .T. ) ;
#19064 = VERTEX_POINT ( 'NONE', #10449 ) ;
#19065 = LINE ( 'NONE', #182, #14280 ) ;
#19066 = DIRECTION ( 'NONE',  ( -0.7739085681710395903, -0.4468163201617135760, -0.4487991802004505648 ) ) ;
#19067 = CARTESIAN_POINT ( 'NONE',  ( -2.528458586775709893, 77.37584602520038857, -3.922623763562873123 ) ) ;
#19068 = ORIENTED_EDGE ( 'NONE', *, *, #9008, .T. ) ;
#19069 = ORIENTED_EDGE ( 'NONE', *, *, #19748, .F. ) ;
#19070 = PLANE ( 'NONE',  #16982 ) ;
#19071 = DIRECTION ( 'NONE',  ( -0.05035489893516267162, -0.02907241445523285617, 0.9983081582712687307 ) ) ;
#19072 = CARTESIAN_POINT ( 'NONE',  ( -12.10766532132493367, 50.39772591864724660, -15.93512085822366231 ) ) ;
#19073 = DIRECTION ( 'NONE',  ( 0.5000000000000055511, -0.8660254037844354880, 0.000000000000000000 ) ) ;
#19074 = AXIS2_PLACEMENT_3D ( 'NONE', #6435, #14648, #3173 ) ;
#19075 = VERTEX_POINT ( 'NONE', #825 ) ;
#19076 = ORIENTED_EDGE ( 'NONE', *, *, #12550, .T. ) ;
#19077 = DIRECTION ( 'NONE',  ( -0.8660254037844354880, -0.5000000000000055511, 0.000000000000000000 ) ) ;
#19079 = EDGE_CURVE ( 'NONE', #15072, #17245, #6487, .T. ) ;
#19078 = CARTESIAN_POINT ( 'NONE',  ( 192.7522908873522738, 17.31795696490239678, -4.003039906353937916 ) ) ;
#19080 = CARTESIAN_POINT ( 'NONE',  ( 59.39721438298058587, 215.0773763115390125, -5.999999999999973355 ) ) ;
#19081 = CARTESIAN_POINT ( 'NONE',  ( 217.7814145706309432, 37.50692764314506178, -12.10162843130809662 ) ) ;
#19082 = CARTESIAN_POINT ( 'NONE',  ( 67.15136315568796022, 72.45226458839093198, -23.16931136300337357 ) ) ;
#19083 = CARTESIAN_POINT ( 'NONE',  ( 229.6708229000879840, 36.58739926862691760, -13.96059298729450759 ) ) ;
#19084 = LINE ( 'NONE', #6232, #20896 ) ;
#19085 = FACE_OUTER_BOUND ( 'NONE', #3985, .T. ) ;
#19086 = AXIS2_PLACEMENT_3D ( 'NONE', #12444, #14036, #2893 ) ;
#19087 = EDGE_CURVE ( 'NONE', #15321, #9010, #8970, .T. ) ;
#19088 = CARTESIAN_POINT ( 'NONE',  ( 205.5965122587965084, 9.994899983462953941, -14.00000000000005507 ) ) ;
#19089 = LINE ( 'NONE', #8031, #18141 ) ;
#19090 = CARTESIAN_POINT ( 'NONE',  ( 219.1487326806684734, 35.13866320645098540, -9.756613004592562532 ) ) ;
#19091 = EDGE_CURVE ( 'NONE', #3379, #8080, #15473, .T. ) ;
#19092 = ORIENTED_EDGE ( 'NONE', *, *, #13159, .F. ) ;
#19093 = CARTESIAN_POINT ( 'NONE',  ( 82.18628316260415545, 64.02363915056508858, 0.4670741050950639739 ) ) ;
#19094 = ORIENTED_EDGE ( 'NONE', *, *, #17329, .T. ) ;
#19095 = ORIENTED_EDGE ( 'NONE', *, *, #17085, .F. ) ;
#19096 = CARTESIAN_POINT ( 'NONE',  ( -3.215901834620719768, 75.81673797945757087, -2.071606702244279674 ) ) ;
#19097 = CARTESIAN_POINT ( 'NONE',  ( -14.99999999999999645, -10.00000000000000000, 15.00000000000000000 ) ) ;
#19098 = DIRECTION ( 'NONE',  ( -0.9795788631971381610, 0.000000000000000000, 0.2010603162670408506 ) ) ;
#19099 = ITEM_DEFINED_TRANSFORMATION ( 'NONE', 'NONE', #18572,  #18233 ) ;
#19100 = AXIS2_PLACEMENT_3D ( 'NONE', #13469, #19918, #17927 ) ;
#19101 = VECTOR ( 'NONE', #12833, 1000.000000000000114 ) ;
#19102 = DIRECTION ( 'NONE',  ( -0.5000000000000006661, 6.009258394948590704E-18, 0.8660254037844382635 ) ) ;
#19103 = VERTEX_POINT ( 'NONE', #10345 ) ;
#19104 = PRODUCT_DEFINITION ( 'UNKNOWN', '', #11817, #4288 ) ;
#19105 = CARTESIAN_POINT ( 'NONE',  ( 213.9187556984697380, 7.376742007230097542, -24.25943249057096907 ) ) ;
#19106 = CARTESIAN_POINT ( 'NONE',  ( 205.2612434495831621, 1.115232799514996209, -14.00000000000005507 ) ) ;
#19107 = LINE ( 'NONE', #17620, #1216 ) ;
#19108 = CARTESIAN_POINT ( 'NONE',  ( 0.2950380200214504645, 60.04495121932129820, 1.663291502479429251 ) ) ;
#19109 = ADVANCED_FACE ( 'NONE', ( #7271 ), #1999, .T. ) ;
#19110 = DIRECTION ( 'NONE',  ( 0.000000000000000000, 0.000000000000000000, -1.000000000000000000 ) ) ;
#19111 = CARTESIAN_POINT ( 'NONE',  ( 220.2180084519553134, 35.41797800104779270, -14.00000000000005507 ) ) ;
#19112 = ADVANCED_FACE ( 'NONE', ( #16833 ), #15268, .F. ) ;
#19113 = CARTESIAN_POINT ( 'NONE',  ( 215.9737506317248119, 15.45515208972567756, -9.718744748713270099 ) ) ;
#19114 = DIRECTION ( 'NONE',  ( 1.000000000000000000, 0.000000000000000000, 0.000000000000000000 ) ) ;
#19115 = DIRECTION ( 'NONE',  ( 0.4814586436739045072, -0.8339108325863955340, -0.2697967711570115057 ) ) ;
#19116 = VERTEX_POINT ( 'NONE', #17247 ) ;
#19117 = DIRECTION ( 'NONE',  ( 0.2961981327260175267, 0.1710100716628331352, -0.9396926207859105373 ) ) ;
#19118 = EDGE_CURVE ( 'NONE', #17847, #11795, #1035, .T. ) ;
#19119 = CARTESIAN_POINT ( 'NONE',  ( -15.99999999999999289, 80.00000000000000000, -4.999999999999993783 ) ) ;
#19120 = FACE_OUTER_BOUND ( 'NONE', #18829, .T. ) ;
#19121 = CARTESIAN_POINT ( 'NONE',  ( -18.48100260771138537, 20.09941697557067641, 4.999999999999990230 ) ) ;
#19122 = DIRECTION ( 'NONE',  ( -1.000000000000000000, 0.000000000000000000, 0.000000000000000000 ) ) ;
#19124 = ORIENTED_EDGE ( 'NONE', *, *, #8891, .T. ) ;
#19123 = ORIENTED_EDGE ( 'NONE', *, *, #873, .T. ) ;
#19125 = EDGE_CURVE ( 'NONE', #6033, #8359, #11826, .T. ) ;
#19126 =( LENGTH_UNIT ( ) NAMED_UNIT ( * ) SI_UNIT ( .MILLI., .METRE. ) );
#19127 = CARTESIAN_POINT ( 'NONE',  ( -15.99999999999999289, 80.00000000000000000, 4.999999999999993783 ) ) ;
#19128 = FACE_OUTER_BOUND ( 'NONE', #6499, .T. ) ;
#19129 = EDGE_CURVE ( 'NONE', #9937, #7814, #2461, .T. ) ;
#19130 = CARTESIAN_POINT ( 'NONE',  ( 229.3079840454082330, 36.88936454335567561, -15.95040389705438777 ) ) ;
#19131 = ADVANCED_FACE ( 'NONE', ( #10769 ), #18843, .T. ) ;
#19132 = ORIENTED_EDGE ( 'NONE', *, *, #13893, .F. ) ;
#19133 = CARTESIAN_POINT ( 'NONE',  ( 37.00490953756720813, 229.8619860023653132, 26.00000000000001776 ) ) ;
#19134 = DIRECTION ( 'NONE',  ( 0.000000000000000000, 0.8660254037844380415, -0.5000000000000009992 ) ) ;
#19135 = EDGE_CURVE ( 'NONE', #13669, #7321, #14232, .T. ) ;
#19136 = ADVANCED_FACE ( 'NONE', ( #4319 ), #13761, .F. ) ;
#19137 = DIRECTION ( 'NONE',  ( 0.5000000000000026645, -0.8660254037844370423, 0.000000000000000000 ) ) ;
#19138 = CARTESIAN_POINT ( 'NONE',  ( 31.00000000000000711, 65.00000000000000000, -25.50000000000000000 ) ) ;
#19139 = ORIENTED_EDGE ( 'NONE', *, *, #11445, .T. ) ;
#19140 = DIRECTION ( 'NONE',  ( 0.6946590618905486014, 0.4010615963775267523, 0.5971585917027842916 ) ) ;
#19141 = EDGE_CURVE ( 'NONE', #1190, #6217, #18423, .T. ) ;
#19142 = ORIENTED_EDGE ( 'NONE', *, *, #18603, .F. ) ;
#19143 = ORIENTED_EDGE ( 'NONE', *, *, #1210, .F. ) ;
#19144 = AXIS2_PLACEMENT_3D ( 'NONE', #15933, #18237, #11457 ) ;
#19145 = DIRECTION ( 'NONE',  ( 0.8426815769442658199, 0.4865224352899169546, -0.2306158707424407761 ) ) ;
#19146 = DIRECTION ( 'NONE',  ( 0.000000000000000000, -1.000000000000000000, 0.000000000000000000 ) ) ;
#19147 = CARTESIAN_POINT ( 'NONE',  ( 4.000000000000000000, 3.518949890710767026, -4.987329993433320396E-15 ) ) ;
#19148 = DIRECTION ( 'NONE',  ( 0.000000000000000000, -0.6317949158655086217, -0.7751355909042590975 ) ) ;
#19149 =( NAMED_UNIT ( * ) PLANE_ANGLE_UNIT ( ) SI_UNIT ( $, .RADIAN. ) );
#19150 = ADVANCED_FACE ( 'NONE', ( #15778 ), #17246, .T. ) ;
#19151 = ORIENTED_EDGE ( 'NONE', *, *, #12865, .F. ) ;
#19152 = CIRCLE ( 'NONE', #3227, 4.999999999999998224 ) ;
#19153 = DIRECTION ( 'NONE',  ( -0.7951984747223628247, -0.4591080534401421609, -0.3960797660391544572 ) ) ;
#19154 = AXIS2_PLACEMENT_3D ( 'NONE', #19097, #4570, #11036 ) ;
#19155 = DIRECTION ( 'NONE',  ( -0.8660254037844357100, -0.5000000000000051070, 0.000000000000000000 ) ) ;
#19156 = CARTESIAN_POINT ( 'NONE',  ( -5.258301051201804910, 51.04712924960224285, -6.516085000401124816 ) ) ;
#19157 = DIRECTION ( 'NONE',  ( -0.4758887346169382027, -0.2747544890354036706, 0.8354878114129395961 ) ) ;
#19158 = VECTOR ( 'NONE', #18451, 1000.000000000000114 ) ;
#19159 = EDGE_CURVE ( 'NONE', #2247, #14942, #7514, .T. ) ;
#19160 = CARTESIAN_POINT ( 'NONE',  ( 64.99529059433392320, 211.3812238888322952, 16.00000000000001066 ) ) ;
#19161 = CARTESIAN_POINT ( 'NONE',  ( 98.77092417049759376, 200.0087193835544497, 13.49999999999999822 ) ) ;
#19162 = B_SPLINE_CURVE_WITH_KNOTS ( 'NONE', 3,
 ( #18605, #15136, #18397, #16907 ),
 .UNSPECIFIED., .F., .F.,
 ( 4, 4 ),
 ( 5.392423665750742885E-07, 0.0008545249803497876294 ),
 .UNSPECIFIED. ) ;
#19164 = ORIENTED_EDGE ( 'NONE', *, *, #11184, .F. ) ;
#19163 = VERTEX_POINT ( 'NONE', #20930 ) ;
#19165 = CARTESIAN_POINT ( 'NONE',  ( 5.000000000000004441, 2.342598717236899830, -4.057500000000030305 ) ) ;
#19166 = CARTESIAN_POINT ( 'NONE',  ( 213.2304086110926278, 13.87128283563446018, -4.915515517929359035 ) ) ;
#19167 = CARTESIAN_POINT ( 'NONE',  ( -3.376929201035539840, 76.35052269458216756, -2.692414605357460466 ) ) ;
#19168 = ORIENTED_EDGE ( 'NONE', *, *, #8821, .T. ) ;
#19169 = ORIENTED_EDGE ( 'NONE', *, *, #15491, .T. ) ;
#19170 = ORIENTED_EDGE ( 'NONE', *, *, #4592, .F. ) ;
#19171 = CARTESIAN_POINT ( 'NONE',  ( 206.6134256523022259, 3.931827829199530999, -26.28791492288515386 ) ) ;
#19172 = LINE ( 'NONE', #10899, #9484 ) ;
#19173 = CARTESIAN_POINT ( 'NONE',  ( -32.22615568004599851, 60.40488302444183688, 1.799529103756865478 ) ) ;
#19174 = VECTOR ( 'NONE', #19051, 1000.000000000000114 ) ;
#19175 = DIRECTION ( 'NONE',  ( 0.000000000000000000, 0.000000000000000000, 1.000000000000000000 ) ) ;
#19176 = VERTEX_POINT ( 'NONE', #9591 ) ;
#19177 = ORIENTED_EDGE ( 'NONE', *, *, #10551, .F. ) ;
#19178 = VECTOR ( 'NONE', #11086, 1000.000000000000227 ) ;
#19179 = CARTESIAN_POINT ( 'NONE',  ( -0.03591081202477939410, 67.75983095507352516, 2.252573492070593986 ) ) ;
#19180 = CIRCLE ( 'NONE', #1912, 19.99999999999999645 ) ;
#19181 = EDGE_CURVE ( 'NONE', #570, #10573, #14905, .T. ) ;
#19182 = DIRECTION ( 'NONE',  ( 0.8660254037844370423, 0.5000000000000027756, -6.106226635438360972E-16 ) ) ;
#19183 = LINE ( 'NONE', #2969, #16996 ) ;
#19184 = CARTESIAN_POINT ( 'NONE',  ( -27.39676811513723109, 61.45283151330974647, 5.134886483425054493 ) ) ;
#19185 = CARTESIAN_POINT ( 'NONE',  ( 79.66744006002031142, 66.27074226415487601, -25.44098493566588459 ) ) ;
#19186 = EDGE_LOOP ( 'NONE', ( #11109, #12557, #10537, #3797, #8895, #6791 ) ) ;
#19187 = CARTESIAN_POINT ( 'NONE',  ( 227.3339954826201392, 40.96137216016710170, -10.64970491435233413 ) ) ;
#19188 = DIRECTION ( 'NONE',  ( 0.000000000000000000, 0.000000000000000000, 1.000000000000000000 ) ) ;
#19189 = DIRECTION ( 'NONE',  ( 0.000000000000000000, 0.000000000000000000, -1.000000000000000000 ) ) ;
#19190 = VECTOR ( 'NONE', #19544, 1000.000000000000114 ) ;
#19191 = ORIENTED_EDGE ( 'NONE', *, *, #8242, .F. ) ;
#19192 = CARTESIAN_POINT ( 'NONE',  ( 81.96607779882778289, 65.76354676051263937, 0.6364889541190595912 ) ) ;
#19193 = ORIENTED_EDGE ( 'NONE', *, *, #7216, .T. ) ;
#19194 = EDGE_CURVE ( 'NONE', #8955, #8547, #9106, .T. ) ;
#19195 = ORIENTED_EDGE ( 'NONE', *, *, #4975, .T. ) ;
#19196 = LINE ( 'NONE', #9532, #13572 ) ;
#19197 = PLANE ( 'NONE',  #17161 ) ;
#19198 = PRODUCT_CONTEXT ( 'NONE', #123, 'mechanical' ) ;
#19199 = CARTESIAN_POINT ( 'NONE',  ( 209.7177441667290339, 12.37429433490069997, -24.99940654434242759 ) ) ;
#19200 = ORIENTED_EDGE ( 'NONE', *, *, #5586, .F. ) ;
#19201 = AXIS2_PLACEMENT_3D ( 'NONE', #3064, #1169, #7617 ) ;
#19202 = B_SPLINE_CURVE_WITH_KNOTS ( 'NONE', 3,
 ( #10636, #20289, #5755, #1122 ),
 .UNSPECIFIED., .F., .F.,
 ( 4, 4 ),
 ( 0.0004399335472996286221, 0.0008623086312854339732 ),
 .UNSPECIFIED. ) ;
#19203 = DIRECTION ( 'NONE',  ( 0.8660254037844355990, 0.5000000000000054401, 0.000000000000000000 ) ) ;
#19204 = ADVANCED_FACE ( 'NONE', ( #17675 ), #12797, .F. ) ;
#19205 = ADVANCED_BREP_SHAPE_REPRESENTATION ( '', ( #17741, #18233 ), #20925 ) ;
#19206 = AXIS2_PLACEMENT_3D ( 'NONE', #12626, #11127, #4351 ) ;
#19207 = DIRECTION ( 'NONE',  ( -0.8660254037844361541, -0.5000000000000044409, 5.976026924694052093E-17 ) ) ;
#19208 = CARTESIAN_POINT ( 'NONE',  ( 0.000000000000000000, 7.715274834628324392E-16, -6.099999999999999645 ) ) ;
#19209 = CARTESIAN_POINT ( 'NONE',  ( 5.000000000000004441, 0.000000000000000000, 0.000000000000000000 ) ) ;
#19210 = LINE ( 'NONE', #5082, #1218 ) ;
#19211 = FACE_OUTER_BOUND ( 'NONE', #17273, .T. ) ;
#19212 = CARTESIAN_POINT ( 'NONE',  ( 208.0154570403101104, 11.39147840422468150, -16.96430480073851399 ) ) ;
#19213 = CARTESIAN_POINT ( 'NONE',  ( 209.3909370991932519, 3.422763374394458769, -14.00000000000005507 ) ) ;
#19214 = LINE ( 'NONE', #4586, #13598 ) ;
#19215 = DIRECTION ( 'NONE',  ( 0.5000000000000049960, -0.8660254037844358210, 0.000000000000000000 ) ) ;
#19216 = ORIENTED_EDGE ( 'NONE', *, *, #15660, .T. ) ;
#19217 = FACE_OUTER_BOUND ( 'NONE', #17132, .T. ) ;
#19218 = CARTESIAN_POINT ( 'NONE',  ( 82.60162025600570246, 64.43303002238135946, 0.6088031877440995832 ) ) ;
#19219 = EDGE_CURVE ( 'NONE', #6001, #3962, #16087, .T. ) ;
#19220 = MECHANICAL_DESIGN_GEOMETRIC_PRESENTATION_REPRESENTATION (  '', ( #13819 ), #7035 ) ;
#19221 = LINE ( 'NONE', #7868, #10814 ) ;
#19222 = CARTESIAN_POINT ( 'NONE',  ( 37.85427444295662269, 178.3908428320656299, 11.00000000000001243 ) ) ;
#19223 = AXIS2_PLACEMENT_3D ( 'NONE', #16574, #14901, #1952 ) ;
#19225 = EDGE_LOOP ( 'NONE', ( #6552, #20385, #8638, #1080 ) ) ;
#19224 = VERTEX_POINT ( 'NONE', #1248 ) ;
#19226 = ORIENTED_EDGE ( 'NONE', *, *, #7148, .F. ) ;
#19227 = CARTESIAN_POINT ( 'NONE',  ( 218.4336835101095460, 38.50851945753705508, -15.57898118447794822 ) ) ;
#19228 = ORIENTED_EDGE ( 'NONE', *, *, #16161, .F. ) ;
#19229 = EDGE_CURVE ( 'NONE', #6453, #9959, #14611, .T. ) ;
#19230 = FACE_OUTER_BOUND ( 'NONE', #7813, .T. ) ;
#19231 = ORIENTED_EDGE ( 'NONE', *, *, #8711, .F. ) ;
#19232 = LINE ( 'NONE', #9769, #11433 ) ;
#19233 = EDGE_CURVE ( 'NONE', #15281, #6173, #3992, .T. ) ;
#19234 = CARTESIAN_POINT ( 'NONE',  ( -28.16330156462496603, 79.99999999984028420, -2.903060217166834267 ) ) ;
#19235 = CARTESIAN_POINT ( 'NONE',  ( 208.0983737146324870, 5.661548828456886895, -14.00000000000005507 ) ) ;
#19236 = AXIS2_PLACEMENT_3D ( 'NONE', #15431, #12126, #13937 ) ;
#19237 = FACE_OUTER_BOUND ( 'NONE', #13340, .T. ) ;
#19238 = EDGE_CURVE ( 'NONE', #1853, #6314, #18144, .T. ) ;
#19239 = ORIENTED_EDGE ( 'NONE', *, *, #9145, .F. ) ;
#19240 = DIRECTION ( 'NONE',  ( 0.3200921998322428519, -0.5544159532159279591, -0.7682212795973759611 ) ) ;
#19241 = CARTESIAN_POINT ( 'NONE',  ( 205.8894739819445761, 2.741034046794848855, -25.34310559273324159 ) ) ;
#19242 = LINE ( 'NONE', #14591, #10820 ) ;
#19243 = CARTESIAN_POINT ( 'NONE',  ( 222.0097383132401490, 32.10863278189405179, -13.51727824498698283 ) ) ;
#19244 = VERTEX_POINT ( 'NONE', #1347 ) ;
#19245 = CARTESIAN_POINT ( 'NONE',  ( 59.39721438298058587, 215.0773763115390125, -22.00000000000000355 ) ) ;
#19246 = EDGE_CURVE ( 'NONE', #11760, #2644, #6204, .T. ) ;
#19247 = VERTEX_POINT ( 'NONE', #5991 ) ;
#19248 = CIRCLE ( 'NONE', #10080, 9.999999999999998224 ) ;
#19249 = CARTESIAN_POINT ( 'NONE',  ( 211.4089818235499365, 27.46411299765594904, -13.67111640670284167 ) ) ;
#19250 = CARTESIAN_POINT ( 'NONE',  ( 201.4958824572256333, 7.627400263678961068, -2.990331769139143780 ) ) ;
#19251 = PLANE ( 'NONE',  #5285 ) ;
#19252 = EDGE_CURVE ( 'NONE', #6453, #1337, #13526, .T. ) ;
#19253 = DIRECTION ( 'NONE',  ( -0.000000000000000000, 1.295896757998782163E-15, 1.000000000000000000 ) ) ;
#19254 = DIRECTION ( 'NONE',  ( -0.8660254037844358210, -0.5000000000000049960, 0.000000000000000000 ) ) ;
#19255 = ORIENTED_EDGE ( 'NONE', *, *, #17292, .F. ) ;
#19256 = CARTESIAN_POINT ( 'NONE',  ( 227.5312376355471145, 39.64027283883993391, -14.00000000000005507 ) ) ;
#19257 = EDGE_CURVE ( 'NONE', #20124, #16739, #7084, .T. ) ;
#19258 = ADVANCED_FACE ( 'NONE', ( #6096 ), #9276, .F. ) ;
#19259 = VECTOR ( 'NONE', #678, 1000.000000000000000 ) ;
#19260 =( LENGTH_UNIT ( ) NAMED_UNIT ( * ) SI_UNIT ( .MILLI., .METRE. ) );
#19261 = CARTESIAN_POINT ( 'NONE',  ( -5.379344836516867900, 50.95069562376034611, -6.689558405576774724 ) ) ;
#19262 = CARTESIAN_POINT ( 'NONE',  ( 221.0683110530012527, 31.81385593646023935, -13.56204498775467115 ) ) ;
#19263 = PRODUCT_DEFINITION_FORMATION_WITH_SPECIFIED_SOURCE ( 'ANY', '', #783, .NOT_KNOWN. ) ;
#19264 = CARTESIAN_POINT ( 'NONE',  ( 199.4425753138606296, -0.2082645440182918917, -20.84195174293567376 ) ) ;
#19265 = LINE ( 'NONE', #14405, #2245 ) ;
#19266 = ORIENTED_EDGE ( 'NONE', *, *, #16940, .T. ) ;
#19267 = VERTEX_POINT ( 'NONE', #12590 ) ;
#19268 = DIRECTION ( 'NONE',  ( -0.5000000000000045519, 0.8660254037844360431, 0.000000000000000000 ) ) ;
#19269 = DIRECTION ( 'NONE',  ( 1.000000000000000000, 0.000000000000000000, 0.000000000000000000 ) ) ;
#19270 = ADVANCED_FACE ( 'NONE', ( #6305 ), #7694, .T. ) ;
#19271 = CARTESIAN_POINT ( 'NONE',  ( -11.94919551499654808, 80.00000000000871125, -11.83620004860075703 ) ) ;
#19272 = ORIENTED_EDGE ( 'NONE', *, *, #7870, .T. ) ;
#19273 = ORIENTED_EDGE ( 'NONE', *, *, #14886, .T. ) ;
#19274 = ORIENTED_EDGE ( 'NONE', *, *, #20007, .T. ) ;
#19275 = CARTESIAN_POINT ( 'NONE',  ( 229.6917281522317751, 36.87765938573448921, -12.97935860811667652 ) ) ;
#19276 = LINE ( 'NONE', #7777, #15629 ) ;
#19277 = CARTESIAN_POINT ( 'NONE',  ( -33.09260109148557660, 56.28423912749347835, -0.2677176956847754363 ) ) ;
#19278 = DIRECTION ( 'NONE',  ( -0.5000000000000054401, 0.8660254037844354880, -0.000000000000000000 ) ) ;
#19279 = VERTEX_POINT ( 'NONE', #2939 ) ;
#19280 = AXIS2_PLACEMENT_3D ( 'NONE', #957, #18660, #4451 ) ;
#19281 = ORIENTED_EDGE ( 'NONE', *, *, #10975, .F. ) ;
#19282 = CARTESIAN_POINT ( 'NONE',  ( 8.399999999999998579, 0.000000000000000000, -4.400000000000000355 ) ) ;
#19283 = EDGE_CURVE ( 'NONE', #6269, #19267, #2984, .T. ) ;
#19284 = FACE_OUTER_BOUND ( 'NONE', #12351, .T. ) ;
#19285 = DIRECTION ( 'NONE',  ( 0.8660254037844355990, 0.5000000000000054401, 8.899770914925154148E-15 ) ) ;
#19286 = FACE_OUTER_BOUND ( 'NONE', #18653, .T. ) ;
#19287 = LINE ( 'NONE', #9625, #6858 ) ;
#19288 = AXIS2_PLACEMENT_3D ( 'NONE', #3586, #4868, #11756 ) ;
#19289 = CARTESIAN_POINT ( 'NONE',  ( -28.72625095155510522, 68.32062926339966680, 2.141136792363286911 ) ) ;
#19290 = DIRECTION ( 'NONE',  ( 0.000000000000000000, 0.000000000000000000, -1.000000000000000000 ) ) ;
#19291 = DIRECTION ( 'NONE',  ( 0.8660254037844360431, 0.5000000000000044409, -5.976026924694052093E-17 ) ) ;
#19292 = VERTEX_POINT ( 'NONE', #3036 ) ;
#19293 = CARTESIAN_POINT ( 'NONE',  ( 58.85476768585063923, 85.28574669046319912, -10.58199671080212489 ) ) ;
#19294 = VECTOR ( 'NONE', #9283, 1000.000000000000227 ) ;
#19295 = ORIENTED_EDGE ( 'NONE', *, *, #20399, .F. ) ;
#19296 = ORIENTED_EDGE ( 'NONE', *, *, #9251, .T. ) ;
#19297 = CARTESIAN_POINT ( 'NONE',  ( 221.4018633254588622, 31.23612645358364048, -14.58164069303003529 ) ) ;
#19298 = CARTESIAN_POINT ( 'NONE',  ( 228.6212422746358186, 38.73179531451560109, -10.33191597617941326 ) ) ;
#19299 = CARTESIAN_POINT ( 'NONE',  ( 82.49529059433407951, 181.0703347563770365, 11.00000000000001066 ) ) ;
#19300 = APPLICATION_PROTOCOL_DEFINITION ( 'draft international standard', 'automotive_design', 1998, #17060 ) ;
#19301 = CARTESIAN_POINT ( 'NONE',  ( 210.0930887352476759, 12.05995036078138583, -25.46066938576263894 ) ) ;
#19302 = ORIENTED_EDGE ( 'NONE', *, *, #15653, .T. ) ;
#19303 = SURFACE_STYLE_FILL_AREA ( #12848 ) ;
#19304 = DIRECTION ( 'NONE',  ( 0.5000000000000037748, -0.8660254037844364872, 0.000000000000000000 ) ) ;
#19305 = CARTESIAN_POINT ( 'NONE',  ( 208.9252846479952836, 31.76596812687403926, -14.32921182609460864 ) ) ;
#19306 = DIRECTION ( 'NONE',  ( -1.000000000000000000, 0.000000000000000000, 0.000000000000000000 ) ) ;
#19307 = DIRECTION ( 'NONE',  ( 0.8660254037844370423, 0.5000000000000027756, 1.850371707708595943E-15 ) ) ;
#19308 = DIRECTION ( 'NONE',  ( -0.3412765716093336121, 0.5911083614602787861, 0.7308359642781161458 ) ) ;
#19309 = CIRCLE ( 'NONE', #7486, 5.000000000000008882 ) ;
#19310 = DIRECTION ( 'NONE',  ( 0.8528685319524387243, 0.4924038765061080070, -0.1736481776669413502 ) ) ;
#19311 = CARTESIAN_POINT ( 'NONE',  ( 0.000000000000000000, 0.000000000000000000, 0.000000000000000000 ) ) ;
#19312 = CYLINDRICAL_SURFACE ( 'NONE', #3753, 5.000000000000005329 ) ;
#19313 = VERTEX_POINT ( 'NONE', #11723 ) ;
#19314 = AXIS2_PLACEMENT_3D ( 'NONE', #623, #13666, #13455 ) ;
#19315 = FACE_OUTER_BOUND ( 'NONE', #2699, .T. ) ;
#19316 = CARTESIAN_POINT ( 'NONE',  ( 81.10655718899290889, 54.43739570252013493, -2.927339837283823520 ) ) ;
#19317 = EDGE_CURVE ( 'NONE', #7993, #15193, #13211, .T. ) ;
#19318 = DIRECTION ( 'NONE',  ( -0.8660254037844361541, -0.5000000000000042188, 0.000000000000000000 ) ) ;
#19319 = CIRCLE ( 'NONE', #6106, 12.47473710546057823 ) ;
#19320 = DIRECTION ( 'NONE',  ( 0.5000000000000045519, -0.8660254037844359321, 0.000000000000000000 ) ) ;
#19322 = VERTEX_POINT ( 'NONE', #8637 ) ;
#19321 = ORIENTED_EDGE ( 'NONE', *, *, #18884, .T. ) ;
#19323 = AXIS2_PLACEMENT_3D ( 'NONE', #10780, #9287, #17474 ) ;
#19324 =( NAMED_UNIT ( * ) SI_UNIT ( $, .STERADIAN. ) SOLID_ANGLE_UNIT ( ) );
#19325 = EDGE_LOOP ( 'NONE', ( #14182, #15150, #20150, #13443 ) ) ;
#19326 = B_SPLINE_CURVE_WITH_KNOTS ( 'NONE', 3,
 ( #4951, #14738, #14840, #6736 ),
 .UNSPECIFIED., .F., .F.,
 ( 4, 4 ),
 ( 4.013812776577353094E-06, 0.0004560670545564213881 ),
 .UNSPECIFIED. ) ;
#19327 = DIRECTION ( 'NONE',  ( -0.8660254037844360431, -0.5000000000000045519, -4.336808689942049784E-16 ) ) ;
#19328 = ORIENTED_EDGE ( 'NONE', *, *, #5390, .T. ) ;
#19329 = CARTESIAN_POINT ( 'NONE',  ( 218.8636229293586837, 35.63248778145287332, -9.834987871251028579 ) ) ;
#19330 = CARTESIAN_POINT ( 'NONE',  ( -32.28295608689890628, 78.37037279069637918, -5.691146419800033662 ) ) ;
#19331 = CARTESIAN_POINT ( 'NONE',  ( 198.4821375217713353, 5.887413813925527428, -22.72623880687287468 ) ) ;
#19332 = VECTOR ( 'NONE', #3178, 999.9999999999998863 ) ;
#19333 = VERTEX_POINT ( 'NONE', #9897 ) ;
#19334 = EDGE_CURVE ( 'NONE', #16824, #7395, #13345, .T. ) ;
#19335 = VECTOR ( 'NONE', #19408, 1000.000000000000000 ) ;
#19336 = CARTESIAN_POINT ( 'NONE',  ( 42.39721438298049350, 244.5222400402098231, -8.999999999999973355 ) ) ;
#19337 = AXIS2_PLACEMENT_3D ( 'NONE', #9471, #10755, #12787 ) ;
#19338 = FACE_OUTER_BOUND ( 'NONE', #9161, .T. ) ;
#19339 = CARTESIAN_POINT ( 'NONE',  ( 162.0049095375683237, 13.35563505625637859, -14.00000000000000355 ) ) ;
#19340 = ORIENTED_EDGE ( 'NONE', *, *, #13714, .T. ) ;
#19341 = CARTESIAN_POINT ( 'NONE',  ( 193.6508758837858011, 7.222081524111755968, -19.95367855226118081 ) ) ;
#19342 = ADVANCED_FACE ( 'NONE', ( #384 ), #8784, .T. ) ;
#19343 = FACE_OUTER_BOUND ( 'NONE', #7711, .T. ) ;
#19344 = EDGE_CURVE ( 'NONE', #11275, #7000, #13319, .T. ) ;
#19345 = ORIENTED_EDGE ( 'NONE', *, *, #4362, .F. ) ;
#19346 = CARTESIAN_POINT ( 'NONE',  ( 5.000000000000000000, 0.000000000000000000, 0.000000000000000000 ) ) ;
#19347 = EDGE_LOOP ( 'NONE', ( #19063, #19541, #5179, #10018, #7665 ) ) ;
#19348 = DIRECTION ( 'NONE',  ( 0.7071067811865432429, 0.000000000000000000, -0.7071067811865517916 ) ) ;
#19349 = DIRECTION ( 'NONE',  ( -0.5000000000000049960, 0.8660254037844358210, -0.000000000000000000 ) ) ;
#19350 = CONICAL_SURFACE ( 'NONE', #6465, 10.85470691220533190, 0.8171114040043576665 ) ;
#19351 = AXIS2_PLACEMENT_3D ( 'NONE', #3815, #2135, #16860 ) ;
#19352 = EDGE_CURVE ( 'NONE', #570, #14413, #13007, .T. ) ;
#19353 = DIRECTION ( 'NONE',  ( 0.000000000000000000, 1.000000000000000000, 0.000000000000000000 ) ) ;
#19354 = PLANE ( 'NONE',  #7018 ) ;
#19355 = ORIENTED_EDGE ( 'NONE', *, *, #618, .T. ) ;
#19356 = CARTESIAN_POINT ( 'NONE',  ( -34.00000000000000711, 65.00000000000000000, -12.50000000000000000 ) ) ;
#19357 = EDGE_CURVE ( 'NONE', #5157, #15623, #3461, .T. ) ;
#19358 = VERTEX_POINT ( 'NONE', #19661 ) ;
#19359 = CARTESIAN_POINT ( 'NONE',  ( -4.864993619586824636, 45.51589215631262419, -5.690233592220027781 ) ) ;
#19360 = DIRECTION ( 'NONE',  ( -0.8660254037844372643, -0.5000000000000024425, 0.000000000000000000 ) ) ;
#19361 = VECTOR ( 'NONE', #1738, 1000.000000000000000 ) ;
#19362 = EDGE_CURVE ( 'NONE', #2667, #16542, #11490, .T. ) ;
#19363 = CARTESIAN_POINT ( 'NONE',  ( 220.5256391327309302, 34.26729766263312627, -17.38313153181864834 ) ) ;
#19364 = VECTOR ( 'NONE', #10881, 1000.000000000000000 ) ;
#19365 = DIRECTION ( 'NONE',  ( -0.8660254037844355990, -0.5000000000000051070, 0.000000000000000000 ) ) ;
#19367 = ORIENTED_EDGE ( 'NONE', *, *, #1008, .T. ) ;
#19366 = ORIENTED_EDGE ( 'NONE', *, *, #15245, .F. ) ;
#19368 = ORIENTED_EDGE ( 'NONE', *, *, #2394, .F. ) ;
#19369 = CARTESIAN_POINT ( 'NONE',  ( 196.7640869814540565, 9.019494789394645551, -5.407152407593843968 ) ) ;
#19370 = LINE ( 'NONE', #13119, #12231 ) ;
#19371 = CARTESIAN_POINT ( 'NONE',  ( -12.38627653609458257, 79.99792423946917097, -12.24236967450151958 ) ) ;
#19372 = EDGE_LOOP ( 'NONE', ( #6015, #17725, #7733, #14930, #2619, #13151 ) ) ;
#19373 = ORIENTED_EDGE ( 'NONE', *, *, #3990, .F. ) ;
#19374 = ORIENTED_EDGE ( 'NONE', *, *, #1350, .F. ) ;
#19375 = DIRECTION ( 'NONE',  ( 1.000000000000000000, -0.000000000000000000, 0.000000000000000000 ) ) ;
#19376 = CARTESIAN_POINT ( 'NONE',  ( 214.6548693368118848, 14.87071829951450930, -7.229707551136565158 ) ) ;
#19377 = DIRECTION ( 'NONE',  ( -0.5000000000000049960, 0.8660254037844357100, -0.000000000000000000 ) ) ;
#19378 = DIRECTION ( 'NONE',  ( -0.000000000000000000, 0.000000000000000000, 1.000000000000000000 ) ) ;
#19379 = ORIENTED_EDGE ( 'NONE', *, *, #19344, .T. ) ;
#19380 = EDGE_CURVE ( 'NONE', #5809, #9819, #16487, .T. ) ;
#19381 = ORIENTED_EDGE ( 'NONE', *, *, #6930, .F. ) ;
#19382 = DIRECTION ( 'NONE',  ( 0.7743856023693594937, 0.000000000000000000, -0.6327139470906613106 ) ) ;
#19383 = AXIS2_PLACEMENT_3D ( 'NONE', #6772, #10267, #3704 ) ;
#19384 =( GEOMETRIC_REPRESENTATION_CONTEXT ( 3 ) GLOBAL_UNCERTAINTY_ASSIGNED_CONTEXT ( ( #5962 ) ) GLOBAL_UNIT_ASSIGNED_CONTEXT ( ( #19886, #17039, #11742 ) ) REPRESENTATION_CONTEXT ( 'NONE', 'WORKASPACE' ) );
#19385 = CARTESIAN_POINT ( 'NONE',  ( 59.65554463217813463, 240.6299351947967011, -13.99999999999998046 ) ) ;
#19386 = ADVANCED_FACE ( 'NONE', ( #18505 ), #12040, .F. ) ;
#19387 = CARTESIAN_POINT ( 'NONE',  ( 72.00490953756758472, 169.2402077374547957, 11.00000000000001243 ) ) ;
#19388 = CARTESIAN_POINT ( 'NONE',  ( 63.16228553181007754, 74.18705481243415534, -21.71006526367976974 ) ) ;
#19389 = ORIENTED_EDGE ( 'NONE', *, *, #6417, .F. ) ;
#19390 = CARTESIAN_POINT ( 'NONE',  ( 44.00000000000000000, 0.000000000000000000, -15.00000000000000355 ) ) ;
#19391 = DIRECTION ( 'NONE',  ( 0.8660254037844370423, 0.5000000000000026645, -0.000000000000000000 ) ) ;
#19392 = VERTEX_POINT ( 'NONE', #17518 ) ;
#19393 = ADVANCED_FACE ( 'NONE', ( #19005 ), #11699, .T. ) ;
#19394 = AXIS2_PLACEMENT_3D ( 'NONE', #17251, #2421, #828 ) ;
#19395 = CARTESIAN_POINT ( 'NONE',  ( 61.20179353631819907, 75.03121440969175637, -4.223626890520874255 ) ) ;
#19396 = ORIENTED_EDGE ( 'NONE', *, *, #13033, .T. ) ;
#19397 = CARTESIAN_POINT ( 'NONE',  ( 221.2721513107338183, 32.94427583580249319, -11.64051170696124338 ) ) ;
#19398 = DIRECTION ( 'NONE',  ( -0.8660254037844359321, -0.5000000000000045519, 5.976026924694053325E-17 ) ) ;
#19399 = ADVANCED_FACE ( 'NONE', ( #20088 ), #17798, .F. ) ;
#19400 = CARTESIAN_POINT ( 'NONE',  ( 208.0983737146324870, 5.661548828456886895, -14.00000000000005507 ) ) ;
#19401 = EDGE_LOOP ( 'NONE', ( #14946, #839, #20704, #18740, #3596 ) ) ;
#19402 = EDGE_CURVE ( 'NONE', #8219, #4596, #10943, .T. ) ;
#19403 = CARTESIAN_POINT ( 'NONE',  ( 209.9679726729889921, 12.16473724899237041, -25.30691987834803669 ) ) ;
#19404 = ORIENTED_EDGE ( 'NONE', *, *, #10268, .T. ) ;
#19405 = DIRECTION ( 'NONE',  ( -0.8660254037844380415, -0.5000000000000014433, -0.000000000000000000 ) ) ;
#19406 = CIRCLE ( 'NONE', #3502, 1.000000000000000888 ) ;
#19407 = CARTESIAN_POINT ( 'NONE',  ( 211.0319935650719572, 27.94071137980556685, -15.65309054528693089 ) ) ;
#19408 = DIRECTION ( 'NONE',  ( 0.000000000000000000, -0.4999999999999987232, 0.8660254037844393737 ) ) ;
#19409 = CARTESIAN_POINT ( 'NONE',  ( 221.8613199550661363, 32.36570091902735413, -15.54214587067338016 ) ) ;
#19410 = DIRECTION ( 'NONE',  ( 0.8660254037844380415, 0.5000000000000014433, 0.000000000000000000 ) ) ;
#19411 = FACE_OUTER_BOUND ( 'NONE', #16103, .T. ) ;
#19412 = DIRECTION ( 'NONE',  ( 0.000000000000000000, -1.000000000000000000, 1.355657144061424088E-15 ) ) ;
#19413 = DIRECTION ( 'NONE',  ( 0.5016613886297202063, 0.000000000000000000, -0.8650640734408641119 ) ) ;
#19414 = VERTEX_POINT ( 'NONE', #4481 ) ;
#19415 = ORIENTED_EDGE ( 'NONE', *, *, #12418, .T. ) ;
#19416 = CARTESIAN_POINT ( 'NONE',  ( 227.9553588074475670, 39.88513931160575510, -14.00000000000005507 ) ) ;
#19417 = DIRECTION ( 'NONE',  ( 0.000000000000000000, -1.000000000000000000, 0.000000000000000000 ) ) ;
#19418 = CARTESIAN_POINT ( 'NONE',  ( 9.999999999999994671, 0.000000000000000000, 0.000000000000000000 ) ) ;
#19419 = CIRCLE ( 'NONE', #136, 3.902363844300875240 ) ;
#19420 = CARTESIAN_POINT ( 'NONE',  ( 79.90495664118901686, 50.99637491787829902, -18.20149439789049239 ) ) ;
#19421 = VECTOR ( 'NONE', #760, 1000.000000000000114 ) ;
#19423 = EDGE_LOOP ( 'NONE', ( #5797, #20168, #1527, #3735 ) ) ;
#19422 = EDGE_LOOP ( 'NONE', ( #17237, #10222 ) ) ;
#19424 =( NAMED_UNIT ( * ) PLANE_ANGLE_UNIT ( ) SI_UNIT ( $, .RADIAN. ) );
#19425 = VERTEX_POINT ( 'NONE', #2286 ) ;
#19426 = CARTESIAN_POINT ( 'NONE',  ( -33.07802712247563193, 73.66227117401376745, -0.2439945722892326863 ) ) ;
#19427 = ORIENTED_EDGE ( 'NONE', *, *, #14796, .T. ) ;
#19428 = DIRECTION ( 'NONE',  ( -0.8660254037844354880, -0.5000000000000055511, 0.000000000000000000 ) ) ;
#19429 = ADVANCED_FACE ( 'NONE', ( #13524 ), #11938, .F. ) ;
#19430 = CARTESIAN_POINT ( 'NONE',  ( 209.9266392777186923, 12.49489998346296638, -2.187257959407756136 ) ) ;
#19431 = CARTESIAN_POINT ( 'NONE',  ( 78.37318721450539272, 67.09492480576284379, 0.3327101687020665444 ) ) ;
#19432 = DIRECTION ( 'NONE',  ( 0.8660254037844368202, 0.5000000000000031086, -0.000000000000000000 ) ) ;
#19433 = ORIENTED_EDGE ( 'NONE', *, *, #5620, .F. ) ;
#19434 = PLANE ( 'NONE',  #14593 ) ;
#19435 = ORIENTED_EDGE ( 'NONE', *, *, #1060, .T. ) ;
#19436 = LINE ( 'NONE', #4916, #8845 ) ;
#19437 = EDGE_CURVE ( 'NONE', #11977, #11320, #2891, .T. ) ;
#19438 = ORIENTED_EDGE ( 'NONE', *, *, #15677, .T. ) ;
#19439 = DIRECTION ( 'NONE',  ( 0.6048098792058536066, 0.000000000000000000, 0.7963698952214358640 ) ) ;
#19440 = CARTESIAN_POINT ( 'NONE',  ( 0.000000000000000000, -2.342598717236910932, -4.057499999999996554 ) ) ;
#19441 = CARTESIAN_POINT ( 'NONE',  ( 162.0049095375683237, 13.35563505625637859, -9.000000000000005329 ) ) ;
#19442 = CARTESIAN_POINT ( 'NONE',  ( -33.48481952675158624, 80.00000000000001421, 0.7287565553229297111 ) ) ;
#19443 = CARTESIAN_POINT ( 'NONE',  ( -29.99999999999996447, 5.000000000000006217, -9.730120459829299406 ) ) ;
#19444 = DIRECTION ( 'NONE',  ( 0.8660254037844371533, 0.5000000000000025535, 6.106226635438359986E-16 ) ) ;
#19445 = EDGE_CURVE ( 'NONE', #20929, #7471, #802, .T. ) ;
#19446 = ORIENTED_EDGE ( 'NONE', *, *, #19845, .T. ) ;
#19447 = B_SPLINE_CURVE_WITH_KNOTS ( 'NONE', 3,
 ( #7397, #12819, #94, #18103, #1783, #16107, #12922, #8225, #6525, #3159, #6629, #4947, #5152, #9914, #3569, #13123, #11639, #10015, #8333, #1884, #16508, #17692 ),
 .UNSPECIFIED., .F., .F.,
 ( 4, 2, 2, 2, 2, 2, 2, 2, 2, 2, 4 ),
 ( 0.000000000000000000, 0.002138836336596521351, 0.003208254504894782026, 0.004277672673193042702, 0.004812381757342181279, 0.005347090841491319857, 0.006416509009789597880, 0.006951218093938736457, 0.007485927178087873300, 0.008020636262237011010, 0.008555345346386149588 ),
 .UNSPECIFIED. ) ;
#19448 = ADVANCED_FACE ( 'NONE', ( #590 ), #16808, .F. ) ;
#19449 = CARTESIAN_POINT ( 'NONE',  ( 77.32469725096443369, 69.07004555494354747, -24.89440563207301693 ) ) ;
#19450 = CARTESIAN_POINT ( 'NONE',  ( -11.12092984962295539, 45.32949789690962206, -11.51493324710881971 ) ) ;
#19451 = CARTESIAN_POINT ( 'NONE',  ( -6.842857967119176266, 50.10839126059149606, -14.33286777257530709 ) ) ;
#19452 = CARTESIAN_POINT ( 'NONE',  ( 0.6607651890765847691, 78.07072705852067429, -5.138138717405499101 ) ) ;
#19453 = DIRECTION ( 'NONE',  ( 0.1503837331804444843, 0.08682408883347161876, 0.9848077530122060219 ) ) ;
#19454 = CARTESIAN_POINT ( 'NONE',  ( 218.2832399571946667, 38.76909533485677173, -13.49489896056980420 ) ) ;
#19455 = CONICAL_SURFACE ( 'NONE', #12428, 14.99999999999999645, 0.7853981633974543852 ) ;
#19457 = ORIENTED_EDGE ( 'NONE', *, *, #7473, .T. ) ;
#19456 = ORIENTED_EDGE ( 'NONE', *, *, #9899, .F. ) ;
#19458 = VERTEX_POINT ( 'NONE', #12143 ) ;
#19459 = LINE ( 'NONE', #3465, #5758 ) ;
#19460 = DIRECTION ( 'NONE',  ( 0.000000000000000000, 0.000000000000000000, -1.000000000000000000 ) ) ;
#19461 = VERTEX_POINT ( 'NONE', #20290 ) ;
#19462 = PRODUCT_RELATED_PRODUCT_CATEGORY ( 'part', '', ( #5672 ) ) ;
#19463 = CARTESIAN_POINT ( 'NONE',  ( 229.5966506884888645, 36.71586930762607182, -12.96012118015705994 ) ) ;
#19464 = LINE ( 'NONE', #16203, #10159 ) ;
#19465 = DIRECTION ( 'NONE',  ( 0.000000000000000000, 1.000000000000000000, -1.295896757998782163E-15 ) ) ;
#19466 = DIRECTION ( 'NONE',  ( -1.000000000000000000, 0.000000000000000000, -0.000000000000000000 ) ) ;
#19467 = EDGE_LOOP ( 'NONE', ( #454, #5745, #5741, #16436, #15562 ) ) ;
#19468 = ORIENTED_EDGE ( 'NONE', *, *, #13951, .T. ) ;
#19469 = FACE_OUTER_BOUND ( 'NONE', #2009, .T. ) ;
#19470 = AXIS2_PLACEMENT_3D ( 'NONE', #5463, #8440, #720 ) ;
#19471 = EDGE_CURVE ( 'NONE', #9396, #19458, #19162, .T. ) ;
#19472 = AXIS2_PLACEMENT_3D ( 'NONE', #1091, #5939, #7645 ) ;
#19473 = ADVANCED_FACE ( 'NONE', ( #1302 ), #14778, .T. ) ;
#19474 = AXIS2_PLACEMENT_3D ( 'NONE', #4583, #5757, #2996 ) ;
#19475 = CARTESIAN_POINT ( 'NONE',  ( 218.2368265400617133, 38.23163736213975028, -12.98880265512657672 ) ) ;
#19476 = LINE ( 'NONE', #4959, #1099 ) ;
#19477 = CARTESIAN_POINT ( 'NONE',  ( -28.66803663422406601, 63.25105461977041443, 2.419216852106436999 ) ) ;
#19478 = CARTESIAN_POINT ( 'NONE',  ( -20.83667610223213629, 16.40927555158100759, 11.52655978026935024 ) ) ;
#19479 =( REPRESENTATION_RELATIONSHIP ('NONE','NONE', #4634, #20602 ) REPRESENTATION_RELATIONSHIP_WITH_TRANSFORMATION ( #16539 )SHAPE_REPRESENTATION_RELATIONSHIP( ) );
#19480 = ORIENTED_EDGE ( 'NONE', *, *, #8290, .T. ) ;
#19481 = DIRECTION ( 'NONE',  ( -0.6048098792058536066, 0.000000000000000000, -0.7963698952214358640 ) ) ;
#19482 = CARTESIAN_POINT ( 'NONE',  ( 27.66668267600675435, 65.75000000000001421, 1.813692929321165437 ) ) ;
#19483 = EDGE_CURVE ( 'NONE', #5859, #1000, #4080, .T. ) ;
#19484 = ORIENTED_EDGE ( 'NONE', *, *, #675, .T. ) ;
#19485 = CARTESIAN_POINT ( 'NONE',  ( 62.17876964677807905, 78.42404429838002500, -11.53082529887307395 ) ) ;
#19486 = ORIENTED_EDGE ( 'NONE', *, *, #19402, .T. ) ;
#19487 = CIRCLE ( 'NONE', #2584, 3.902363844300875240 ) ;
#19488 = CARTESIAN_POINT ( 'NONE',  ( 218.8737197432240293, 10.23749183229395676, -11.23040475586419085 ) ) ;
#19489 = CIRCLE ( 'NONE', #14112, 3.902363844300875240 ) ;
#19490 = CARTESIAN_POINT ( 'NONE',  ( 229.4660061303077327, 36.28915550503100462, -13.49489896056993743 ) ) ;
#19491 = EDGE_CURVE ( 'NONE', #10603, #6779, #10553, .T. ) ;
#19492 = B_SPLINE_CURVE_WITH_KNOTS ( 'NONE', 3,
 ( #19811, #9843, #10259, #5281 ),
 .UNSPECIFIED., .F., .F.,
 ( 4, 4 ),
 ( 3.993865398787763773E-07, 0.0006730501785855516356 ),
 .UNSPECIFIED. ) ;
#19493 = ORIENTED_EDGE ( 'NONE', *, *, #7877, .T. ) ;
#19494 = CARTESIAN_POINT ( 'NONE',  ( -14.99999999999999645, 5.000000000000000000, -15.00000000000000000 ) ) ;
#19495 = CONTEXT_DEPENDENT_SHAPE_REPRESENTATION ( #13400, #7020 ) ;
#19496 = ADVANCED_FACE ( 'NONE', ( #17623 ), #11355, .T. ) ;
#19497 = LINE ( 'NONE', #7947, #7897 ) ;
#19498 = VERTEX_POINT ( 'NONE', #3299 ) ;
#19499 = VECTOR ( 'NONE', #9352, 1000.000000000000000 ) ;
#19500 = DIRECTION ( 'NONE',  ( 0.000000000000000000, -0.000000000000000000, -1.000000000000000000 ) ) ;
#19501 = CARTESIAN_POINT ( 'NONE',  ( 211.8034485311565049, 13.57847631115287435, -23.60546391700164648 ) ) ;
#19502 = AXIS2_PLACEMENT_3D ( 'NONE', #18837, #17560, #4311 ) ;
#19503 = CYLINDRICAL_SURFACE ( 'NONE', #3914, 19.99999999999999645 ) ;
#19504 = CARTESIAN_POINT ( 'NONE',  ( 218.1634319850578549, 38.35624038801824298, -13.96731517339622286 ) ) ;
#19505 = EDGE_CURVE ( 'NONE', #11547, #17982, #6665, .T. ) ;
#19506 = FACE_OUTER_BOUND ( 'NONE', #19372, .T. ) ;
#19507 = DIRECTION ( 'NONE',  ( 1.000000000000000000, 0.000000000000000000, 0.000000000000000000 ) ) ;
#19508 = FACE_OUTER_BOUND ( 'NONE', #6813, .T. ) ;
#19509 = ADVANCED_FACE ( 'NONE', ( #23 ), #17731, .F. ) ;
#19510 = ORIENTED_EDGE ( 'NONE', *, *, #16664, .T. ) ;
#19511 = ORIENTED_EDGE ( 'NONE', *, *, #19711, .F. ) ;
#19512 = CARTESIAN_POINT ( 'NONE',  ( -15.99999999999999289, 80.00000000000000000, 0.000000000000000000 ) ) ;
#19513 = CARTESIAN_POINT ( 'NONE',  ( 60.04195699026302435, 84.37304789033045438, -8.186064125905904376 ) ) ;
#19514 = CARTESIAN_POINT ( 'NONE',  ( -11.71793669819365569, 66.46870624085923396, -2.582219875156729127 ) ) ;
#19515 = CARTESIAN_POINT ( 'NONE',  ( 78.10850005371658256, 52.36126203026114467, -15.57772792125065919 ) ) ;
#19516 = EDGE_CURVE ( 'NONE', #1208, #11547, #19210, .T. ) ;
#19518 = ORIENTED_EDGE ( 'NONE', *, *, #15875, .F. ) ;
#19517 = ORIENTED_EDGE ( 'NONE', *, *, #12999, .T. ) ;
#19519 = VERTEX_POINT ( 'NONE', #12854 ) ;
#19520 = VECTOR ( 'NONE', #4183, 1000.000000000000227 ) ;
#19521 = CIRCLE ( 'NONE', #1264, 12.47473710546057823 ) ;
#19522 = ORIENTED_EDGE ( 'NONE', *, *, #36, .T. ) ;
#19523 = VERTEX_POINT ( 'NONE', #7954 ) ;
#19524 = DIRECTION ( 'NONE',  ( -0.5000000000000054401, 0.8660254037844354880, -0.000000000000000000 ) ) ;
#19525 = ORIENTED_EDGE ( 'NONE', *, *, #91, .F. ) ;
#19526 = PLANE ( 'NONE',  #6676 ) ;
#19527 = ADVANCED_FACE ( 'NONE', ( #9546 ), #6277, .T. ) ;
#19528 = CARTESIAN_POINT ( 'NONE',  ( -31.50431546803533678, 78.79719334215234028, -6.605250029488051844 ) ) ;
#19529 = DIRECTION ( 'NONE',  ( -1.000000000000000000, -0.000000000000000000, -0.000000000000000000 ) ) ;
#19530 = CARTESIAN_POINT ( 'NONE',  ( 167.3972143829816446, 28.01588909410086004, -14.00000000000007461 ) ) ;
#19531 = CARTESIAN_POINT ( 'NONE',  ( 81.06711713768373784, 65.00000000000000000, 0.4999999999999962252 ) ) ;
#19532 = CIRCLE ( 'NONE', #5300, 3.902363844300875240 ) ;
#19533 = CARTESIAN_POINT ( 'NONE',  ( 226.4502034873433445, 42.49214479930887478, -16.48323849494058635 ) ) ;
#19534 = VERTEX_POINT ( 'NONE', #8262 ) ;
#19535 = B_SPLINE_CURVE_WITH_KNOTS ( 'NONE', 3,
 ( #7245, #8733, #13628, #15127, #18598, #18178, #4068, #14910, #5325, #20080, #6826, #13411, #19859, #11715, #16035, #9536, #20872, #1601, #20284, #1005, #15, #9044, #1396, #7345, #13944, #9428, #13835, #6450, #12735, #5746, #12639, #18709 ),
 .UNSPECIFIED., .F., .F.,
 ( 4, 2, 2, 2, 2, 2, 2, 2, 2, 2, 2, 2, 2, 2, 2, 4 ),
 ( 0.000000000000000000, 0.0007065482847658889143, 0.001413096569531777829, 0.002826193139063555657, 0.003532741423829438825, 0.004239289708595322427, 0.005652386278127087896, 0.007065482847658845558, 0.008478579417190603221, 0.01130477255625412202, 0.01271786912578587794, 0.01413096569531763214, 0.01695715883438114399, 0.01978335197344465238, 0.02119644854297641004, 0.02260954511250816423 ),
 .UNSPECIFIED. ) ;
#19536 = CARTESIAN_POINT ( 'NONE',  ( -15.99999999999999289, 80.00000000000000000, 0.000000000000000000 ) ) ;
#19538 = CARTESIAN_POINT ( 'NONE',  ( 5.000000000000004441, 7.027796151710827388, -4.057500000000009877 ) ) ;
#19537 = VECTOR ( 'NONE', #17547, 1000.000000000000114 ) ;
#19539 = EDGE_LOOP ( 'NONE', ( #15045, #17846, #19340, #5511, #12952, #8210, #1565, #16476, #20723, #8701, #19988, #10767, #5244, #5571, #17169, #5769, #12272, #14, #7214, #703, #11528, #4386, #11428, #16538, #18263, #20897, #1777, #4822, #3604, #8546, #12028, #10328, #6324, #1112, #257, #14111, #11836, #706, #4234, #4308, #6166, #7806, #10789, #16166, #3469, #18907, #20509, #7642, #18470, #8520, #5982, #5476, #20633, #13354, #20467, #10072, #6992, #13353, #11176, #8730, #11593, #6413, #16251, #7365, #19366, #13522, #19883, #1261, #18647, #20536, #19969, #8604, #9286, #13795, #7251, #7264, #18435, #1836, #17351, #4041, #10174, #20325, #17207, #3447, #306, #20386, #17038, #16943, #7038, #185, #5352, #15177, #11925, #18431, #1162, #9854, #9572, #8248, #20188, #2277, #9935, #5483, #11905, #15582, #11062, #10199, #16104, #3622 ) ) ;
#19540 = LINE ( 'NONE', #11492, #2763 ) ;
#19541 = ORIENTED_EDGE ( 'NONE', *, *, #7849, .F. ) ;
#19542 = LINE ( 'NONE', #158, #2812 ) ;
#19543 = DIRECTION ( 'NONE',  ( -0.000000000000000000, -1.000000000000000000, -0.000000000000000000 ) ) ;
#19544 = DIRECTION ( 'NONE',  ( 0.4895420438411641761, -0.8479116923740015466, -0.2034560130526309463 ) ) ;
#19545 = DIRECTION ( 'NONE',  ( 0.8660254037844360431, 0.5000000000000044409, 0.000000000000000000 ) ) ;
#19546 = AXIS2_PLACEMENT_3D ( 'NONE', #7690, #15775, #18940 ) ;
#19547 = DIRECTION ( 'NONE',  ( -1.000000000000000000, 0.000000000000000000, 9.512199820426880209E-17 ) ) ;
#19548 = VECTOR ( 'NONE', #963, 1000.000000000000114 ) ;
#19549 = CARTESIAN_POINT ( 'NONE',  ( 227.5591259992508526, 39.91847553452564767, -17.80134517191575583 ) ) ;
#19550 = ORIENTED_EDGE ( 'NONE', *, *, #16258, .T. ) ;
#19551 = CIRCLE ( 'NONE', #17544, 11.94520687646042667 ) ;
#19552 = CARTESIAN_POINT ( 'NONE',  ( 67.92197266240974329, 75.00057405452223236, -21.22836514478491665 ) ) ;
#19553 = CARTESIAN_POINT ( 'NONE',  ( -12.20066445503069019, 45.44343745760707520, -11.93361228997413725 ) ) ;
#19554 = ORIENTED_EDGE ( 'NONE', *, *, #7976, .T. ) ;
#19555 = SURFACE_STYLE_FILL_AREA ( #19663 ) ;
#19556 = CARTESIAN_POINT ( 'NONE',  ( 1.121154864378749672, 56.12821655472171756, -0.3994926274425245061 ) ) ;
#19557 = CARTESIAN_POINT ( 'NONE',  ( 205.8264633344831225, 9.596613037118636669, -14.00000000000005507 ) ) ;
#19558 = CARTESIAN_POINT ( 'NONE',  ( 217.7559408036613604, 37.55104950179651979, -15.81459191843834944 ) ) ;
#19559 = DIRECTION ( 'NONE',  ( -0.5000000000000051070, 0.8660254037844359321, -0.000000000000000000 ) ) ;
#19560 = AXIS2_PLACEMENT_3D ( 'NONE', #19735, #7117, #16566 ) ;
#19562 = ORIENTED_EDGE ( 'NONE', *, *, #2652, .T. ) ;
#19561 = ORIENTED_EDGE ( 'NONE', *, *, #7606, .F. ) ;
#19563 = ORIENTED_EDGE ( 'NONE', *, *, #8198, .T. ) ;
#19564 = CARTESIAN_POINT ( 'NONE',  ( 218.5943730328090737, 10.59141717271569938, -9.788772202513543519 ) ) ;
#19565 = DIRECTION ( 'NONE',  ( 0.000000000000000000, -0.5000000000000018874, -0.8660254037844374864 ) ) ;
#19566 = AXIS2_PLACEMENT_3D ( 'NONE', #17225, #2712, #17093 ) ;
#19567 = ORIENTED_EDGE ( 'NONE', *, *, #15019, .F. ) ;
#19568 = EDGE_CURVE ( 'NONE', #6947, #12788, #18635, .T. ) ;
#19569 = CARTESIAN_POINT ( 'NONE',  ( 226.6211368133091923, 39.11482588413117867, -14.00000000000005507 ) ) ;
#19570 = DIRECTION ( 'NONE',  ( -0.4586056507527268566, 0.7943282877419068910, -0.3984010898462484462 ) ) ;
#19571 = LINE ( 'NONE', #9814, #6447 ) ;
#19572 = FACE_BOUND ( 'NONE', #14414, .T. ) ;
#19573 = ORIENTED_EDGE ( 'NONE', *, *, #14596, .F. ) ;
#19574 = ORIENTED_EDGE ( 'NONE', *, *, #4592, .T. ) ;
#19575 = CYLINDRICAL_SURFACE ( 'NONE', #13457, 4.000000000000000000 ) ;
#19576 = VERTEX_POINT ( 'NONE', #14770 ) ;
#19577 = VECTOR ( 'NONE', #18591, 1000.000000000000000 ) ;
#19578 = PLANE ( 'NONE',  #10448 ) ;
#19579 = PRODUCT_DEFINITION_FORMATION_WITH_SPECIFIED_SOURCE ( 'ANY', '', #13821, .NOT_KNOWN. ) ;
#19580 = ADVANCED_FACE ( 'NONE', ( #16045 ), #9848, .F. ) ;
#19581 = FACE_OUTER_BOUND ( 'NONE', #18539, .T. ) ;
#19582 = CARTESIAN_POINT ( 'NONE',  ( -28.93726274132100329, 55.68764042281951276, -0.7073738265182815121 ) ) ;
#19583 = CARTESIAN_POINT ( 'NONE',  ( 205.0662616026534693, 10.91332106064940888, -14.00000000000005507 ) ) ;
#19584 = DIRECTION ( 'NONE',  ( -0.8660254037844361541, -0.5000000000000044409, 5.976026924694052093E-17 ) ) ;
#19585 = DIRECTION ( 'NONE',  ( 0.000000000000000000, 6.938893903907177533E-18, 1.000000000000000000 ) ) ;
#19586 = VERTEX_POINT ( 'NONE', #14670 ) ;
#19587 = CARTESIAN_POINT ( 'NONE',  ( 62.80918080339837672, 78.05660606650189948, -12.61805735025731146 ) ) ;
#19588 = EDGE_CURVE ( 'NONE', #18617, #11306, #1709, .T. ) ;
#19589 = ORIENTED_EDGE ( 'NONE', *, *, #17958, .F. ) ;
#19590 = VECTOR ( 'NONE', #18009, 1000.000000000000114 ) ;
#19591 = EDGE_CURVE ( 'NONE', #12774, #11970, #1445, .T. ) ;
#19592 = VERTEX_POINT ( 'NONE', #16234 ) ;
#19593 = CARTESIAN_POINT ( 'NONE',  ( -0.1461903257121275057, 66.50634452888081682, 2.432944671161595185 ) ) ;
#19594 = CARTESIAN_POINT ( 'NONE',  ( 29.50490953756713353, 242.8523670591319785, -13.99999999999994493 ) ) ;
#19595 = ORIENTED_EDGE ( 'NONE', *, *, #315, .T. ) ;
#19596 = CARTESIAN_POINT ( 'NONE',  ( -33.99999999999997868, 65.00000000000000000, -22.50000000000000000 ) ) ;
#19597 = CARTESIAN_POINT ( 'NONE',  ( 218.1243679439584469, 10.57767345991361552, -19.61257667712965258 ) ) ;
#19598 = ADVANCED_FACE ( 'NONE', ( #20884 ), #6563, .F. ) ;
#19599 = ORIENTED_EDGE ( 'NONE', *, *, #11620, .T. ) ;
#19600 = APPLICATION_CONTEXT ( 'automotive_design' ) ;
#19601 = LINE ( 'NONE', #16543, #18927 ) ;
#19602 = DIRECTION ( 'NONE',  ( 0.000000000000000000, 0.000000000000000000, 1.000000000000000000 ) ) ;
#19603 = VECTOR ( 'NONE', #17047, 1000.000000000000000 ) ;
#19604 = CARTESIAN_POINT ( 'NONE',  ( 227.2419885375618094, 41.12073286365736635, -9.992950739179617514 ) ) ;
#19605 = CYLINDRICAL_SURFACE ( 'NONE', #6178, 5.000000000000002665 ) ;
#19606 = ADVANCED_FACE ( 'NONE', ( #13059 ), #19503, .F. ) ;
#19607 = ORIENTED_EDGE ( 'NONE', *, *, #799, .F. ) ;
#19608 = DIRECTION ( 'NONE',  ( -0.000000000000000000, -1.000000000000000000, -0.000000000000000000 ) ) ;
#19609 = VECTOR ( 'NONE', #3351, 1000.000000000000227 ) ;
#19610 = FACE_OUTER_BOUND ( 'NONE', #1044, .T. ) ;
#19611 = CARTESIAN_POINT ( 'NONE',  ( 198.6336827526812669, -1.448098972604089374, -15.39542905462715261 ) ) ;
#19612 = B_SPLINE_CURVE_WITH_KNOTS ( 'NONE', 3,
 ( #13358, #1911, #14757, #11446 ),
 .UNSPECIFIED., .F., .F.,
 ( 4, 4 ),
 ( 1.737996164779797019E-05, 0.0008713656996325849693 ),
 .UNSPECIFIED. ) ;
#19613 = ORIENTED_EDGE ( 'NONE', *, *, #4857, .F. ) ;
#19614 = DIRECTION ( 'NONE',  ( 0.000000000000000000, -6.938893903907175992E-18, -1.000000000000000000 ) ) ;
#19615 = AXIS2_PLACEMENT_3D ( 'NONE', #3514, #16244, #16355 ) ;
#19616 = EDGE_CURVE ( 'NONE', #7423, #16403, #13160, .T. ) ;
#19617 = CARTESIAN_POINT ( 'NONE',  ( 60.17750726585534693, 84.26876177917138477, -7.997657589800953204 ) ) ;
#19618 = DIRECTION ( 'NONE',  ( -0.8660254037844357100, -0.5000000000000051070, 0.000000000000000000 ) ) ;
#19619 = CARTESIAN_POINT ( 'NONE',  ( 79.56530540348451552, 50.06033247906107420, -15.99481843635178535 ) ) ;
#19621 = ORIENTED_EDGE ( 'NONE', *, *, #3282, .T. ) ;
#19620 = ORIENTED_EDGE ( 'NONE', *, *, #14586, .F. ) ;
#19622 = ORIENTED_EDGE ( 'NONE', *, *, #699, .T. ) ;
#19623 = VERTEX_POINT ( 'NONE', #20785 ) ;
#19624 = AXIS2_PLACEMENT_3D ( 'NONE', #19341, #3021, #9680 ) ;
#19625 = EDGE_CURVE ( 'NONE', #16672, #2878, #9437, .T. ) ;
#19626 = VECTOR ( 'NONE', #14404, 1000.000000000000227 ) ;
#19627 = FACE_OUTER_BOUND ( 'NONE', #16290, .T. ) ;
#19628 = EDGE_CURVE ( 'NONE', #8182, #15072, #6261, .T. ) ;
#19629 = ORIENTED_EDGE ( 'NONE', *, *, #18892, .T. ) ;
#19630 = CARTESIAN_POINT ( 'NONE',  ( 219.0593366061551137, 10.34465777807333531, -13.97827067520052147 ) ) ;
#19631 = CARTESIAN_POINT ( 'NONE',  ( 220.5718355850134174, 34.18728306015038498, -10.64970491435236788 ) ) ;
#19632 = EDGE_CURVE ( 'NONE', #4064, #12664, #19810, .T. ) ;
#19633 = CIRCLE ( 'NONE', #5752, 5.000000000000005329 ) ;
#19634 = DIRECTION ( 'NONE',  ( -0.5000000000000054401, 0.8660254037844354880, -0.000000000000000000 ) ) ;
#19635 = DIRECTION ( 'NONE',  ( -0.000000000000000000, 1.000000000000000000, -0.000000000000000000 ) ) ;
#19636 = EDGE_LOOP ( 'NONE', ( #14047, #3114, #897, #6387 ) ) ;
#19637 = VECTOR ( 'NONE', #13196, 1000.000000000000000 ) ;
#19638 = FACE_OUTER_BOUND ( 'NONE', #20308, .T. ) ;
#19639 = CARTESIAN_POINT ( 'NONE',  ( -29.99999999999999645, 10.00000000000000000, 10.50000000000000000 ) ) ;
#19640 = AXIS2_PLACEMENT_3D ( 'NONE', #15763, #10643, #2824 ) ;
#19641 = ORIENTED_EDGE ( 'NONE', *, *, #3850, .F. ) ;
#19642 = DIRECTION ( 'NONE',  ( 0.000000000000000000, -1.000000000000000000, 0.000000000000000000 ) ) ;
#19643 = ADVANCED_FACE ( 'NONE', ( #5392 ), #16861, .F. ) ;
#19644 = CONICAL_SURFACE ( 'NONE', #17968, 4.999999999999995559, 1.029744258676653867 ) ;
#19645 = ORIENTED_EDGE ( 'NONE', *, *, #17031, .T. ) ;
#19646 = FACE_OUTER_BOUND ( 'NONE', #3410, .T. ) ;
#19647 = CARTESIAN_POINT ( 'NONE',  ( 30.00000000000000000, -10.00000000000000000, 30.00000000000000000 ) ) ;
#19648 = CARTESIAN_POINT ( 'NONE',  ( 219.2080768649571496, 11.20335309717537520, -15.43274561385901400 ) ) ;
#19649 = AXIS2_PLACEMENT_3D ( 'NONE', #17123, #5975, #7354 ) ;
#19650 = EDGE_CURVE ( 'NONE', #11656, #15055, #11312, .T. ) ;
#19651 = VECTOR ( 'NONE', #610, 1000.000000000000227 ) ;
#19652 = CARTESIAN_POINT ( 'NONE',  ( 76.71035566961047891, 71.19323729334777795, -25.06553181697876909 ) ) ;
#19653 = CARTESIAN_POINT ( 'NONE',  ( -27.37662084148517039, 9.618015882392517923, -5.189762514993161879 ) ) ;
#19654 = AXIS2_PLACEMENT_3D ( 'NONE', #15832, #20789, #6257 ) ;
#19655 = AXIS2_PLACEMENT_3D ( 'NONE', #4640, #17158, #14311 ) ;
#19656 = DIRECTION ( 'NONE',  ( 1.000000000000000000, 0.000000000000000000, 0.000000000000000000 ) ) ;
#19657 = CARTESIAN_POINT ( 'NONE',  ( 221.0087504897275039, 31.91701785817781811, -12.98880265512673127 ) ) ;
#19658 = ORIENTED_EDGE ( 'NONE', *, *, #7456, .T. ) ;
#19659 = AXIS2_PLACEMENT_3D ( 'NONE', #16822, #2197, #10548 ) ;
#19660 = CARTESIAN_POINT ( 'NONE',  ( 80.43867252173693316, 66.63842558683731454, -25.41598262729068836 ) ) ;
#19661 = CARTESIAN_POINT ( 'NONE',  ( 229.6037303676573629, 37.03007601957109074, -12.62147488791610961 ) ) ;
#19662 = ORIENTED_EDGE ( 'NONE', *, *, #17534, .T. ) ;
#19663 = FILL_AREA_STYLE ('',( #3552 ) ) ;
#19664 = CARTESIAN_POINT ( 'NONE',  ( 1.274666701857165352, 51.86400000113221154, -5.249213278443415120 ) ) ;
#19665 = CARTESIAN_POINT ( 'NONE',  ( -8.643231066280758768, 79.96312735385207304, -11.40287558748652863 ) ) ;
#19666 = FACE_OUTER_BOUND ( 'NONE', #13029, .T. ) ;
#19667 = LINE ( 'NONE', #17991, #11507 ) ;
#19668 = VECTOR ( 'NONE', #5673, 1000.000000000000000 ) ;
#19669 = DIRECTION ( 'NONE',  ( 0.8528685319524408337, 0.4924038765061092282, 0.1736481776669271115 ) ) ;
#19671 = ORIENTED_EDGE ( 'NONE', *, *, #10587, .T. ) ;
#19670 = VERTEX_POINT ( 'NONE', #2343 ) ;
#19672 = ORIENTED_EDGE ( 'NONE', *, *, #17691, .T. ) ;
#19673 = CARTESIAN_POINT ( 'NONE',  ( 188.4856654865874077, 14.85461964123948242, -12.53629070788332278 ) ) ;
#19675 = FACE_OUTER_BOUND ( 'NONE', #18029, .T. ) ;
#19674 = VECTOR ( 'NONE', #12710, 1000.000000000000000 ) ;
#19676 = ORIENTED_EDGE ( 'NONE', *, *, #464, .F. ) ;
#19677 = DIRECTION ( 'NONE',  ( -0.8660254037844378194, -0.5000000000000013323, -0.000000000000000000 ) ) ;
#19678 = CARTESIAN_POINT ( 'NONE',  ( 215.8800731390675764, 9.281929250168950318, -4.915515517929356371 ) ) ;
#19679 = CARTESIAN_POINT ( 'NONE',  ( 229.6243373519787099, 36.99438367573579001, -12.60011953066312529 ) ) ;
#19680 = CARTESIAN_POINT ( 'NONE',  ( -13.43323294362767051, 59.26984403206416374, -4.299749073728320603 ) ) ;
#19681 = ORIENTED_EDGE ( 'NONE', *, *, #6118, .T. ) ;
#19682 = ORIENTED_EDGE ( 'NONE', *, *, #12608, .F. ) ;
#19683 = CARTESIAN_POINT ( 'NONE',  ( 199.3895759864363413, 6.411323655772897645, -23.60546391700144397 ) ) ;
#19684 = B_SPLINE_CURVE_WITH_KNOTS ( 'NONE', 3,
 ( #438, #14977, #6662, #15187 ),
 .UNSPECIFIED., .F., .F.,
 ( 4, 4 ),
 ( 0.0001188559543176825488, 0.0007915067463633553230 ),
 .UNSPECIFIED. ) ;
#19685 = CONICAL_SURFACE ( 'NONE', #10547, 13.07248899748297433, 0.6693469023067423196 ) ;
#19686 = CARTESIAN_POINT ( 'NONE',  ( 216.5552780741873278, 15.79089711517258188, -12.53629070788368338 ) ) ;
#19687 = VECTOR ( 'NONE', #10505, 1000.000000000000114 ) ;
#19688 = VECTOR ( 'NONE', #9036, 1000.000000000000227 ) ;
#19689 = EDGE_CURVE ( 'NONE', #9958, #804, #2229, .T. ) ;
#19690 = DIRECTION ( 'NONE',  ( 0.5000000000000052180, -0.8660254037844355990, -0.000000000000000000 ) ) ;
#19691 = CARTESIAN_POINT ( 'NONE',  ( -28.09246286469363341, 54.35809415438139069, 3.171690999751710205 ) ) ;
#19692 = DIRECTION ( 'NONE',  ( 0.000000000000000000, 6.938893903907177533E-18, 1.000000000000000000 ) ) ;
#19693 = DIRECTION ( 'NONE',  ( -0.8660254037844355990, -0.5000000000000055511, 0.000000000000000000 ) ) ;
#19694 = CARTESIAN_POINT ( 'NONE',  ( 79.17199999999999704, 0.000000000000000000, 0.000000000000000000 ) ) ;
#19695 = ORIENTED_EDGE ( 'NONE', *, *, #20908, .F. ) ;
#19696 = CARTESIAN_POINT ( 'NONE',  ( 64.30665537872349091, 77.16043010324054308, -6.802757212025057676 ) ) ;
#19697 = EDGE_LOOP ( 'NONE', ( #11073, #16201 ) ) ;
#19698 = ORIENTED_EDGE ( 'NONE', *, *, #11877, .T. ) ;
#19699 = CARTESIAN_POINT ( 'NONE',  ( -4.675850232754709346, 67.00845937185172829, 5.293280639217825545 ) ) ;
#19700 = CARTESIAN_POINT ( 'NONE',  ( 226.2284856962982360, 42.87617127834123210, -14.91677899116113082 ) ) ;
#19701 = AXIS2_PLACEMENT_3D ( 'NONE', #9438, #11148, #16144 ) ;
#19702 = EDGE_CURVE ( 'NONE', #3954, #19916, #13395, .T. ) ;
#19703 = CONICAL_SURFACE ( 'NONE', #10206, 13.07248899748297433, 0.6693469023067423196 ) ;
#19704 = ORIENTED_EDGE ( 'NONE', *, *, #1306, .F. ) ;
#19705 = CARTESIAN_POINT ( 'NONE',  ( 5.000000000000000000, -2.342598717236910932, -4.057499999999996554 ) ) ;
#19706 = ITEM_DEFINED_TRANSFORMATION ( 'NONE', 'NONE', #974,  #18233 ) ;
#19707 = CARTESIAN_POINT ( 'NONE',  ( -29.54966092877796413, 65.74999999999997158, 3.021668726329258980 ) ) ;
#19708 = ORIENTED_EDGE ( 'NONE', *, *, #17191, .T. ) ;
#19709 = FACE_OUTER_BOUND ( 'NONE', #3209, .T. ) ;
#19710 = CARTESIAN_POINT ( 'NONE',  ( 0.3999999999999975797, 0.000000000000000000, 0.000000000000000000 ) ) ;
#19711 = EDGE_CURVE ( 'NONE', #16315, #18586, #8975, .T. ) ;
#19712 = ADVANCED_FACE ( 'NONE', ( #1925 ), #7298, .T. ) ;
#19713 = LINE ( 'NONE', #11671, #9318 ) ;
#19714 = DIRECTION ( 'NONE',  ( 0.7739085681710339282, 0.4468163201617103009, -0.4487991802004634434 ) ) ;
#19715 = ORIENTED_EDGE ( 'NONE', *, *, #6308, .T. ) ;
#19716 = B_SPLINE_CURVE_WITH_KNOTS ( 'NONE', 3,
 ( #248, #4808, #1532, #9673 ),
 .UNSPECIFIED., .F., .F.,
 ( 4, 4 ),
 ( 0.0001323875665768755629, 0.0008050383586195956074 ),
 .UNSPECIFIED. ) ;
#19717 = CARTESIAN_POINT ( 'NONE',  ( 218.1243679439584469, 10.57767345991361552, -19.61257667712965258 ) ) ;
#19718 = DIRECTION ( 'NONE',  ( -0.5000000000000049960, 0.8660254037844357100, -0.000000000000000000 ) ) ;
#19719 = LINE ( 'NONE', #4789, #19012 ) ;
#19720 = ORIENTED_EDGE ( 'NONE', *, *, #14471, .F. ) ;
#19721 = CARTESIAN_POINT ( 'NONE',  ( 214.9156946368443926, 7.952324971666334008, -4.494676796018850951 ) ) ;
#19722 = CARTESIAN_POINT ( 'NONE',  ( 201.8619877917642782, 26.37553173410844565, -13.33277734556806138 ) ) ;
#19723 = DIRECTION ( 'NONE',  ( -0.8137976813493685846, -0.4698463103929575446, 0.3420201433256764290 ) ) ;
#19724 = CARTESIAN_POINT ( 'NONE',  ( 75.03434910434744154, 52.00529523017046074, -13.14249383666435200 ) ) ;
#19726 = ORIENTED_EDGE ( 'NONE', *, *, #15377, .F. ) ;
#19725 = ORIENTED_EDGE ( 'NONE', *, *, #10697, .T. ) ;
#19727 = PRODUCT_DEFINITION ( 'UNKNOWN', '', #20938, #6176 ) ;
#19728 = ORIENTED_EDGE ( 'NONE', *, *, #16857, .F. ) ;
#19729 = APPLICATION_CONTEXT ( 'automotive_design' ) ;
#19730 = ORIENTED_EDGE ( 'NONE', *, *, #10551, .T. ) ;
#19731 = CIRCLE ( 'NONE', #8918, 3.902363844300875240 ) ;
#19732 = ADVANCED_FACE ( 'NONE', ( #5185 ), #18478, .T. ) ;
#19733 = CARTESIAN_POINT ( 'NONE',  ( 1.500000000000001332, 5.551115123125782702E-17, 8.000000000000058620 ) ) ;
#19734 = VERTEX_POINT ( 'NONE', #8692 ) ;
#19735 = CARTESIAN_POINT ( 'NONE',  ( 174.9952905943348469, 20.85563505625644609, -14.00000000000000533 ) ) ;
#19736 = CARTESIAN_POINT ( 'NONE',  ( -20.12129706306810917, 79.99650906190643695, -12.16257741986414231 ) ) ;
#19737 = CARTESIAN_POINT ( 'NONE',  ( 41.50490953756720813, 222.0677573683055925, -14.00000000000002842 ) ) ;
#19738 = DIRECTION ( 'NONE',  ( -0.5000000000000045519, 0.8660254037844360431, 0.000000000000000000 ) ) ;
#19739 = EDGE_LOOP ( 'NONE', ( #9850, #8739 ) ) ;
#19740 = EDGE_CURVE ( 'NONE', #2193, #3050, #6562, .T. ) ;
#19741 = CARTESIAN_POINT ( 'NONE',  ( 30.00000000000000355, -10.00000000000000000, -15.00000000000000000 ) ) ;
#19742 = EDGE_CURVE ( 'NONE', #2221, #3576, #10157, .T. ) ;
#19743 = CARTESIAN_POINT ( 'NONE',  ( 64.12703260304576247, 73.76969301591478256, -2.890069931837546680 ) ) ;
#19744 = CARTESIAN_POINT ( 'NONE',  ( 205.0662616026534693, 10.91332106064940888, -14.00000000000005507 ) ) ;
#19745 = ORIENTED_EDGE ( 'NONE', *, *, #18111, .F. ) ;
#19746 = AXIS2_PLACEMENT_3D ( 'NONE', #17094, #10496, #2356 ) ;
#19747 = AXIS2_PLACEMENT_3D ( 'NONE', #6137, #15405, #13797 ) ;
#19748 = EDGE_CURVE ( 'NONE', #4359, #10069, #7098, .T. ) ;
#19749 = DIRECTION ( 'NONE',  ( 0.000000000000000000, 0.000000000000000000, -1.000000000000000000 ) ) ;
#19750 = CYLINDRICAL_SURFACE ( 'NONE', #4417, 2.499999999999997780 ) ;
#19751 = EDGE_CURVE ( 'NONE', #17088, #9882, #14980, .T. ) ;
#19752 = LINE ( 'NONE', #11706, #4454 ) ;
#19753 = CARTESIAN_POINT ( 'NONE',  ( 0.2829560868989292599, 78.37037279069626550, -5.691146419799841816 ) ) ;
#19755 = ORIENTED_EDGE ( 'NONE', *, *, #7680, .F. ) ;
#19754 = ORIENTED_EDGE ( 'NONE', *, *, #5872, .F. ) ;
#19756 = DIRECTION ( 'NONE',  ( 0.1348983855785130803, -0.2336508576809998017, -0.9629172873477991335 ) ) ;
#19757 = CARTESIAN_POINT ( 'NONE',  ( 220.0716363630204739, 35.67150189589299458, -10.10863206319040941 ) ) ;
#19758 = DIRECTION ( 'NONE',  ( 0.5000000000000054401, -0.8660254037844354880, 0.000000000000000000 ) ) ;
#19759 = EDGE_CURVE ( 'NONE', #19523, #19879, #19713, .T. ) ;
#19760 = B_SPLINE_CURVE_WITH_KNOTS ( 'NONE', 3,
 ( #15649, #1116, #7560, #5965 ),
 .UNSPECIFIED., .F., .F.,
 ( 4, 4 ),
 ( 2.252543412725310569E-07, 0.0005857136100808785781 ),
 .UNSPECIFIED. ) ;
#19761 = PLANE ( 'NONE',  #11722 ) ;
#19762 = CARTESIAN_POINT ( 'NONE',  ( -29.99999999999999645, 5.000000000000000888, -10.11947335595186281 ) ) ;
#19763 = DIRECTION ( 'NONE',  ( -0.5000000000000051070, 0.8660254037844359321, -0.000000000000000000 ) ) ;
#19764 = ORIENTED_EDGE ( 'NONE', *, *, #16480, .T. ) ;
#19765 = EDGE_CURVE ( 'NONE', #1958, #16809, #20038, .T. ) ;
#19766 = CARTESIAN_POINT ( 'NONE',  ( 81.74095488896709583, 60.03072944676497258, -24.52915917859159123 ) ) ;
#19767 = CARTESIAN_POINT ( 'NONE',  ( -12.93758089954634372, 45.51191724327595978, -12.14335867266129299 ) ) ;
#19768 = ORIENTED_EDGE ( 'NONE', *, *, #11094, .T. ) ;
#19769 = CARTESIAN_POINT ( 'NONE',  ( 28.00000000000001066, 64.25000000000000000, 1.479896280015810639 ) ) ;
#19770 = CARTESIAN_POINT ( 'NONE',  ( 0.7229626692810823263, 57.94382164277974567, 0.7560164722777046320 ) ) ;
#19771 = CARTESIAN_POINT ( 'NONE',  ( 1.076391949077661669, 77.63996874865388520, -4.412329984541580430 ) ) ;
#19772 = ADVANCED_FACE ( 'NONE', ( #10056 ), #6946, .F. ) ;
#19773 = LINE ( 'NONE', #5239, #8145 ) ;
#19774 = DIRECTION ( 'NONE',  ( 0.000000000000000000, -1.000000000000000000, 1.110768649713242108E-15 ) ) ;
#19775 = FACE_OUTER_BOUND ( 'NONE', #19225, .T. ) ;
#19776 = EDGE_CURVE ( 'NONE', #1900, #14685, #5286, .T. ) ;
#19778 = VERTEX_POINT ( 'NONE', #540 ) ;
#19777 = ORIENTED_EDGE ( 'NONE', *, *, #6183, .F. ) ;
#19779 = ORIENTED_EDGE ( 'NONE', *, *, #20809, .F. ) ;
#19780 = CARTESIAN_POINT ( 'NONE',  ( -20.89897948556633978, 14.09941697557065332, 0.9999999999999991118 ) ) ;
#19781 = CARTESIAN_POINT ( 'NONE',  ( 229.3446640726370731, 37.47879200507496478, -16.31968669809504036 ) ) ;
#19782 = ORIENTED_EDGE ( 'NONE', *, *, #3481, .F. ) ;
#19783 = ORIENTED_EDGE ( 'NONE', *, *, #2917, .T. ) ;
#19784 = SURFACE_STYLE_USAGE ( .BOTH. , #13336 ) ;
#19785 = DIRECTION ( 'NONE',  ( -0.8660254037844370423, -0.5000000000000026645, 0.000000000000000000 ) ) ;
#19786 = DIRECTION ( 'NONE',  ( 0.000000000000000000, 0.000000000000000000, -1.000000000000000000 ) ) ;
#19787 = ORIENTED_EDGE ( 'NONE', *, *, #295, .T. ) ;
#19788 = EDGE_CURVE ( 'NONE', #6578, #10554, #15087, .T. ) ;
#19789 = DIRECTION ( 'NONE',  ( 0.000000000000000000, -0.000000000000000000, -1.000000000000000000 ) ) ;
#19790 = CARTESIAN_POINT ( 'NONE',  ( 199.3883551940873247, 6.233608926798073213, -23.74217242726227894 ) ) ;
#19791 = CARTESIAN_POINT ( 'NONE',  ( 40.35427444295665822, 174.0607158131434176, 11.00000000000001243 ) ) ;
#19792 = EDGE_CURVE ( 'NONE', #13943, #12995, #5820, .T. ) ;
#19793 = VECTOR ( 'NONE', #501, 1000.000000000000000 ) ;
#19794 = LINE ( 'NONE', #16834, #415 ) ;
#19795 = CARTESIAN_POINT ( 'NONE',  ( -28.22952087382082809, 47.05996708829931663, -2.604621190020335764 ) ) ;
#19796 = LINE ( 'NONE', #302, #15020 ) ;
#19797 = CARTESIAN_POINT ( 'NONE',  ( 205.1246204644237423, 9.368426547597012544, -26.29020529591235444 ) ) ;
#19798 = DIRECTION ( 'NONE',  ( -0.8660254037844360431, -0.5000000000000044409, 5.976026924694053325E-17 ) ) ;
#19799 = EDGE_LOOP ( 'NONE', ( #9358, #12465, #7876, #531 ) ) ;
#19800 = CARTESIAN_POINT ( 'NONE',  ( 62.62356228232910382, 78.16510281290661055, -12.41974233461093569 ) ) ;
#19801 = ORIENTED_EDGE ( 'NONE', *, *, #10714, .F. ) ;
#19802 = ORIENTED_EDGE ( 'NONE', *, *, #3804, .F. ) ;
#19803 = EDGE_LOOP ( 'NONE', ( #7737, #2358, #9506, #1554 ) ) ;
#19804 = CARTESIAN_POINT ( 'NONE',  ( 47.02433875312717504, 146.5078255381763483, 41.00000000000001421 ) ) ;
#19805 = VECTOR ( 'NONE', #10653, 1000.000000000000114 ) ;
#19806 = CARTESIAN_POINT ( 'NONE',  ( 5.000000000000004441, 4.685197434473814759, -6.938893903907228378E-15 ) ) ;
#19807 = VECTOR ( 'NONE', #6770, 1000.000000000000000 ) ;
#19808 = ORIENTED_EDGE ( 'NONE', *, *, #14406, .F. ) ;
#19809 = LINE ( 'NONE', #120, #13445 ) ;
#19810 = CIRCLE ( 'NONE', #15442, 11.94520687646042667 ) ;
#19811 = CARTESIAN_POINT ( 'NONE',  ( 214.0936945175409676, 14.36970118611001368, -22.03054070023868860 ) ) ;
#19812 = ORIENTED_EDGE ( 'NONE', *, *, #4682, .T. ) ;
#19813 = DIRECTION ( 'NONE',  ( -0.000000000000000000, 1.000000000000000000, -0.000000000000000000 ) ) ;
#19814 = LINE ( 'NONE', #13367, #12389 ) ;
#19815 = CARTESIAN_POINT ( 'NONE',  ( 96.48038057367227793, 209.3071376747316776, 11.00000000000001066 ) ) ;
#19816 = CARTESIAN_POINT ( 'NONE',  ( 203.0246517772554853, 23.22871929987706707, -14.00000000000005507 ) ) ;
#19817 = AXIS2_PLACEMENT_3D ( 'NONE', #16184, #11193, #14709 ) ;
#19818 = ORIENTED_EDGE ( 'NONE', *, *, #10639, .F. ) ;
#19819 = CARTESIAN_POINT ( 'NONE',  ( 205.8534188064671469, 2.720217581527302642, -2.669358488461094581 ) ) ;
#19820 = FACE_OUTER_BOUND ( 'NONE', #1832, .T. ) ;
#19821 = LINE ( 'NONE', #860, #16644 ) ;
#19822 = VECTOR ( 'NONE', #13465, 1000.000000000000114 ) ;
#19823 = EDGE_CURVE ( 'NONE', #18707, #20933, #1070, .T. ) ;
#19824 = ORIENTED_EDGE ( 'NONE', *, *, #3122, .T. ) ;
#19825 = VECTOR ( 'NONE', #15479, 1000.000000000000000 ) ;
#19826 = CARTESIAN_POINT ( 'NONE',  ( 1.500000000000001332, 4.510281037539699062E-17, 6.500000000000047962 ) ) ;
#19827 = CARTESIAN_POINT ( 'NONE',  ( 202.0446258486138902, 25.79888835193206376, -12.69000053959321939 ) ) ;
#19828 = CARTESIAN_POINT ( 'NONE',  ( 205.9211985038822093, 10.18235767446534012, -26.70731555100845611 ) ) ;
#19829 = CARTESIAN_POINT ( 'NONE',  ( 79.42243514894403233, 49.66913713435425137, -10.50195963986585568 ) ) ;
#19831 = VERTEX_POINT ( 'NONE', #12198 ) ;
#19830 = ORIENTED_EDGE ( 'NONE', *, *, #1917, .T. ) ;
#19832 = ADVANCED_FACE ( 'NONE', ( #10595 ), #4246, .F. ) ;
#19833 = CIRCLE ( 'NONE', #4278, 3.047499999999999876 ) ;
#19834 = VERTEX_POINT ( 'NONE', #17079 ) ;
#19835 = CARTESIAN_POINT ( 'NONE',  ( 218.2868491065612488, 38.76284410478177733, -14.55761806292083982 ) ) ;
#19836 = ORIENTED_EDGE ( 'NONE', *, *, #2933, .T. ) ;
#19837 = CIRCLE ( 'NONE', #10702, 13.49999999999999645 ) ;
#19838 = DIRECTION ( 'NONE',  ( -1.000000000000000000, -0.000000000000000000, -0.000000000000000000 ) ) ;
#19839 = CIRCLE ( 'NONE', #10704, 3.902363844300875240 ) ;
#19840 = DIRECTION ( 'NONE',  ( -0.5000000000000049960, 0.8660254037844357100, -0.000000000000000000 ) ) ;
#19841 = CARTESIAN_POINT ( 'NONE',  ( 0.000000000000000000, -4.685197434473809430, 6.071532165918824830E-15 ) ) ;
#19842 = LINE ( 'NONE', #3946, #5893 ) ;
#19843 = ORIENTED_EDGE ( 'NONE', *, *, #15499, .F. ) ;
#19844 = PLANE ( 'NONE',  #7844 ) ;
#19845 = EDGE_CURVE ( 'NONE', #14490, #3353, #2913, .T. ) ;
#19846 = LINE ( 'NONE', #11285, #419 ) ;
#19847 = DIRECTION ( 'NONE',  ( 0.8660254037844360431, 0.5000000000000044409, 4.336808689942049290E-16 ) ) ;
#19848 = ORIENTED_EDGE ( 'NONE', *, *, #5993, .F. ) ;
#19849 = DIRECTION ( 'NONE',  ( 0.000000000000000000, 1.000000000000000000, 0.000000000000000000 ) ) ;
#19850 = DIRECTION ( 'NONE',  ( 0.05035489893516277571, 0.02907241445523329332, -0.9983081582712688418 ) ) ;
#19851 = AXIS2_PLACEMENT_3D ( 'NONE', #17875, #14601, #12894 ) ;
#19852 = CARTESIAN_POINT ( 'NONE',  ( 209.9266392777186923, 12.49489998346296105, -14.00000000000005507 ) ) ;
#19853 = CARTESIAN_POINT ( 'NONE',  ( -9.066344050852512382, 79.93797039651413172, -11.02074839553305985 ) ) ;
#19854 = EDGE_CURVE ( 'NONE', #6173, #4965, #16969, .T. ) ;
#19855 = ORIENTED_EDGE ( 'NONE', *, *, #10844, .F. ) ;
#19856 = ADVANCED_FACE ( 'NONE', ( #6133 ), #20349, .F. ) ;
#19857 = CARTESIAN_POINT ( 'NONE',  ( 44.00000000000000000, -10.00000000000000000, -15.00000000000000355 ) ) ;
#19858 = DIRECTION ( 'NONE',  ( -0.5000000000000049960, 0.8660254037844358210, -0.000000000000000000 ) ) ;
#19859 = CARTESIAN_POINT ( 'NONE',  ( -31.59797023739843880, 78.75485493504352519, -6.506575737150531502 ) ) ;
#19860 = CARTESIAN_POINT ( 'NONE',  ( 206.3750000662386697, 10.09033354729407428, -26.29020529591238287 ) ) ;
#19861 = CARTESIAN_POINT ( 'NONE',  ( -28.50006506553908281, 8.570624926478151551, 0.3342343741539107738 ) ) ;
#19862 = DIRECTION ( 'NONE',  ( -0.8660254037844360431, -0.5000000000000045519, -4.336808689942049784E-16 ) ) ;
#19863 = ORIENTED_EDGE ( 'NONE', *, *, #5399, .F. ) ;
#19864 = EDGE_CURVE ( 'NONE', #3127, #14739, #18878, .T. ) ;
#19865 = CONICAL_SURFACE ( 'NONE', #5987, 1.499999999999990896, 1.503565061787116353 ) ;
#19866 = CARTESIAN_POINT ( 'NONE',  ( 81.45432710247315811, 55.48820219732827752, -22.83971429442600964 ) ) ;
#19867 = CARTESIAN_POINT ( 'NONE',  ( -3.692367643534749888, 52.45729905868842025, 2.215249628048927111 ) ) ;
#19868 = VECTOR ( 'NONE', #19635, 1000.000000000000000 ) ;
#19869 = ORIENTED_EDGE ( 'NONE', *, *, #3850, .T. ) ;
#19870 = CARTESIAN_POINT ( 'NONE',  ( 215.8300749258796145, 8.480242677682491959, -22.62267072728681327 ) ) ;
#19871 = CARTESIAN_POINT ( 'NONE',  ( -4.388108127469900310, 58.67718948633005027, 4.628796252570745118 ) ) ;
#19872 = CARTESIAN_POINT ( 'NONE',  ( -7.329809494601250641, 79.91878874140672906, -10.93332899582966711 ) ) ;
#19873 = ADVANCED_FACE ( 'NONE', ( #960 ), #4349, .F. ) ;
#19874 = LINE ( 'NONE', #6720, #18319 ) ;
#19875 = FACE_OUTER_BOUND ( 'NONE', #14322, .T. ) ;
#19876 = DIRECTION ( 'NONE',  ( 0.1005394128318207181, 0.05804645706261944010, 0.9932383577419421350 ) ) ;
#19878 = ORIENTED_EDGE ( 'NONE', *, *, #17670, .F. ) ;
#19877 = ORIENTED_EDGE ( 'NONE', *, *, #11454, .T. ) ;
#19879 = VERTEX_POINT ( 'NONE', #10801 ) ;
#19880 = DIRECTION ( 'NONE',  ( -0.5000000000000008882, 0.8660254037844381525, 0.000000000000000000 ) ) ;
#19881 = CARTESIAN_POINT ( 'NONE',  ( 203.6497874834091704, 1.447950443965099421, -24.35247136794729528 ) ) ;
#19882 = ADVANCED_FACE ( 'NONE', ( #2765 ), #15519, .F. ) ;
#19883 = ORIENTED_EDGE ( 'NONE', *, *, #20931, .T. ) ;
#19884 = ORIENTED_EDGE ( 'NONE', *, *, #17445, .T. ) ;
#19885 = VECTOR ( 'NONE', #16255, 999.9999999999998863 ) ;
#19886 =( LENGTH_UNIT ( ) NAMED_UNIT ( * ) SI_UNIT ( .MILLI., .METRE. ) );
#19887 = PRODUCT_DEFINITION_SHAPE ( 'NONE', 'NONE',  #20949 ) ;
#19888 = DIRECTION ( 'NONE',  ( 0.000000000000000000, -1.000000000000000000, 0.000000000000000000 ) ) ;
#19889 = FACE_OUTER_BOUND ( 'NONE', #9130, .T. ) ;
#19890 = ORIENTED_EDGE ( 'NONE', *, *, #15349, .T. ) ;
#19891 = AXIS2_PLACEMENT_3D ( 'NONE', #1331, #19134, #1539 ) ;
#19892 = CARTESIAN_POINT ( 'NONE',  ( 229.4135966341432606, 36.37993141518708740, -15.02729838650899552 ) ) ;
#19893 = CARTESIAN_POINT ( 'NONE',  ( -19.67966358621957923, 69.13720662105420445, -3.389612121674969725 ) ) ;
#19894 = ADVANCED_FACE ( 'NONE', ( #10694 ), #20655, .F. ) ;
#19895 = EDGE_CURVE ( 'NONE', #1475, #2644, #9305, .T. ) ;
#19896 = CARTESIAN_POINT ( 'NONE',  ( 82.49529059433407951, 181.0703347563770365, 11.00000000000001066 ) ) ;
#19897 = VECTOR ( 'NONE', #17096, 1000.000000000000114 ) ;
#19898 = B_SPLINE_CURVE_WITH_KNOTS ( 'NONE', 3,
 ( #202, #2114, #16423, #8564 ),
 .UNSPECIFIED., .F., .F.,
 ( 4, 4 ),
 ( 3.377843907047678752E-07, 0.0006729885764489780845 ),
 .UNSPECIFIED. ) ;
#19899 = DIRECTION ( 'NONE',  ( 0.5000000000000054401, -0.8660254037844354880, 0.000000000000000000 ) ) ;
#19900 = CARTESIAN_POINT ( 'NONE',  ( -31.81916350473495925, 50.47282605692874569, -8.748658904665091995 ) ) ;
#19901 = FACE_OUTER_BOUND ( 'NONE', #10869, .T. ) ;
#19902 = EDGE_CURVE ( 'NONE', #12634, #1760, #18977, .T. ) ;
#19903 = VERTEX_POINT ( 'NONE', #4027 ) ;
#19904 = VECTOR ( 'NONE', #12311, 1000.000000000000227 ) ;
#19905 = LINE ( 'NONE', #6968, #16275 ) ;
#19906 = DIRECTION ( 'NONE',  ( -0.8660254037844380415, -0.5000000000000014433, -0.000000000000000000 ) ) ;
#19908 = ORIENTED_EDGE ( 'NONE', *, *, #2048, .T. ) ;
#19907 = VERTEX_POINT ( 'NONE', #7625 ) ;
#19909 = CARTESIAN_POINT ( 'NONE',  ( 59.05986185621148365, 85.12815607961502451, -15.01156433139877500 ) ) ;
#19910 = ORIENTED_EDGE ( 'NONE', *, *, #11000, .F. ) ;
#19911 = ORIENTED_EDGE ( 'NONE', *, *, #1703, .F. ) ;
#19912 = FACE_OUTER_BOUND ( 'NONE', #15448, .T. ) ;
#19913 = LINE ( 'NONE', #2223, #15455 ) ;
#19914 = EDGE_CURVE ( 'NONE', #7395, #18828, #14121, .T. ) ;
#19915 = AXIS2_PLACEMENT_3D ( 'NONE', #17635, #19122, #14571 ) ;
#19916 = VERTEX_POINT ( 'NONE', #15503 ) ;
#19917 = DIRECTION ( 'NONE',  ( -1.000000000000000000, -0.000000000000000000, -0.000000000000000000 ) ) ;
#19918 = DIRECTION ( 'NONE',  ( 0.8660254037844370423, 0.5000000000000026645, -0.000000000000000000 ) ) ;
#19919 = EDGE_LOOP ( 'NONE', ( #16819, #2488, #11646, #6723 ) ) ;
#19920 = LINE ( 'NONE', #18447, #12505 ) ;
#19921 = CARTESIAN_POINT ( 'NONE',  ( 159.9952905943348469, 46.83639716978957068, 0.9999999999999386047 ) ) ;
#19922 = EDGE_LOOP ( 'NONE', ( #5876, #15642, #4338, #5909, #2034 ) ) ;
#19923 = DIRECTION ( 'NONE',  ( -0.1348983855785064190, 0.2336508576809882831, -0.9629172873478027972 ) ) ;
#19924 = DIRECTION ( 'NONE',  ( 0.8660254037844355990, 0.5000000000000054401, -2.489154677768128945E-14 ) ) ;
#19925 = FACE_BOUND ( 'NONE', #8255, .T. ) ;
#19926 = EDGE_LOOP ( 'NONE', ( #18622, #11269, #4637, #14517, #664 ) ) ;
#19927 = CARTESIAN_POINT ( 'NONE',  ( -32.97264659046876289, 73.17878816827422384, 0.08443632837269006430 ) ) ;
#19928 = DIRECTION ( 'NONE',  ( -1.000000000000000000, 0.000000000000000000, 1.153604387573317816E-16 ) ) ;
#19929 = DIRECTION ( 'NONE',  ( -0.5000000000000054401, 0.8660254037844354880, -0.000000000000000000 ) ) ;
#19930 = AXIS2_PLACEMENT_3D ( 'NONE', #10262, #20036, #8584 ) ;
#19931 = ORIENTED_EDGE ( 'NONE', *, *, #16600, .T. ) ;
#19932 = CARTESIAN_POINT ( 'NONE',  ( 82.29621571355018261, 58.30728878437918183, -0.6895527425001902744 ) ) ;
#19933 = CARTESIAN_POINT ( 'NONE',  ( -2.810302697974978781, 79.49366880382952161, -8.593311550919597863 ) ) ;
#19934 = CARTESIAN_POINT ( 'NONE',  ( 97.00490953756778367, 125.9389375482329569, -29.00000000000002487 ) ) ;
#19935 = CARTESIAN_POINT ( 'NONE',  ( 196.8447511938509535, 4.588041795376833321, -7.229707551136296040 ) ) ;
#19937 = ORIENTED_EDGE ( 'NONE', *, *, #17572, .F. ) ;
#19936 = ORIENTED_EDGE ( 'NONE', *, *, #18207, .T. ) ;
#19938 = CARTESIAN_POINT ( 'NONE',  ( 0.000000000000000000, 0.000000000000000000, 0.000000000000000000 ) ) ;
#19939 = B_SPLINE_CURVE_WITH_KNOTS ( 'NONE', 3,
 ( #126, #6560, #12743, #20683, #6156, #12648, #19108, #11045, #4336, #12303, #2858, #1165, #8986, #17378, #5806, #18759, #14214, #17066, #15895, #7715, #11012, #4232, #2543, #15489, #4127, #14318, #20441, #10581, #9293, #948, #10679, #4440, #1367, #20334, #4544, #17165, #20753, #2752, #20641, #6221, #17481, #19072, #7391, #2958, #2647, #12611, #10787, #7818, #9399, #10900, #18649, #9090, #17267, #9193, #15699, #13882, #15797, #1266, #15589, #1056, #7505, #13997, #5905, #7613, #12405, #18863, #20540, #14103, #12501, #6115, #6011, #18961, #1785, #19277, #7919, #16008, #1677, #9714, #6322, #19173, #4648, #1574, #20847, #14418, #6527, #3161 ),
 .UNSPECIFIED., .F., .F.,
 ( 4, 2, 2, 2, 2, 2, 2, 2, 2, 2, 2, 2, 2, 2, 2, 2, 2, 2, 2, 2, 2, 2, 2, 2, 2, 2, 2, 2, 2, 2, 2, 2, 2, 2, 2, 2, 2, 2, 2, 2, 2, 2, 4 ),
 ( 0.000000000000000000, 0.002349933223531118325, 0.003524899835296677053, 0.004699866447062234914, 0.007049799670593371453, 0.008224766282358929315, 0.009399732894124488911, 0.01174966611765559076, 0.01292463272942114168, 0.01409959934118669087, 0.01527456595295224179, 0.01644953256471779271, 0.01879946578824888415, 0.01997443240001442813, 0.02114939901177997558, 0.02349933223531107049, 0.02467429884707661794, 0.02584926545884216192, 0.02819919868237325336, 0.03054913190590434480, 0.03289906512943543970, 0.03524899835296653461, 0.03759893157649762258, 0.03994886480002871054, 0.04229879802355979157, 0.04699866447062195363, 0.04934859769415304159, 0.05169853091768412956, 0.05404846414121521059, 0.05522343075298075110, 0.05639839736474629162, 0.05874833058827737264, 0.05992329720004292010, 0.06109826381180846061, 0.06344819703533953470, 0.06462316364710508909, 0.06579813025887064348, 0.06814806348240172451, 0.06932303009416727890, 0.07049799670593281942, 0.07284792992946390044, 0.07402289654122945484, 0.07519786315299499535 ),
 .UNSPECIFIED. ) ;
#19940 = CARTESIAN_POINT ( 'NONE',  ( -15.99999999999999289, -9.999999999999994671, 0.000000000000000000 ) ) ;
#19941 = VECTOR ( 'NONE', #20317, 1000.000000000000000 ) ;
#19942 = ORIENTED_EDGE ( 'NONE', *, *, #1872, .F. ) ;
#19943 = CARTESIAN_POINT ( 'NONE',  ( 75.62464799035413421, 52.78861731102380617, -8.028657343369459909 ) ) ;
#19944 = CARTESIAN_POINT ( 'NONE',  ( -18.57603018928663019, 80.00000000000416378, -12.24234612424543478 ) ) ;
#19945 = CARTESIAN_POINT ( 'NONE',  ( 211.7058770681882152, 6.356735158160116583, -25.61390257072256560 ) ) ;
#19946 = LINE ( 'NONE', #12013, #16249 ) ;
#19947 = ORIENTED_EDGE ( 'NONE', *, *, #5489, .F. ) ;
#19948 = LINE ( 'NONE', #15110, #7176 ) ;
#19949 = AXIS2_PLACEMENT_3D ( 'NONE', #7967, #4795, #1419 ) ;
#19950 = DIRECTION ( 'NONE',  ( 0.000000000000000000, 0.000000000000000000, -1.000000000000000000 ) ) ;
#19951 = EDGE_CURVE ( 'NONE', #4749, #13189, #19981, .T. ) ;
#19952 = DIRECTION ( 'NONE',  ( -0.5000000000000042188, 0.8660254037844362651, 0.000000000000000000 ) ) ;
#19953 = ORIENTED_EDGE ( 'NONE', *, *, #4739, .T. ) ;
#19954 = DIRECTION ( 'NONE',  ( -0.5000000000000049960, 0.8660254037844357100, -0.000000000000000000 ) ) ;
#19955 = LINE ( 'NONE', #12124, #18981 ) ;
#19956 = LINE ( 'NONE', #18384, #751 ) ;
#19957 = VECTOR ( 'NONE', #20093, 1000.000000000000000 ) ;
#19958 = CARTESIAN_POINT ( 'NONE',  ( -10.45864600352303420, 79.97447990077584734, -11.55951008316059614 ) ) ;
#19959 = VERTEX_POINT ( 'NONE', #3371 ) ;
#19960 = VECTOR ( 'NONE', #19774, 1000.000000000000000 ) ;
#19961 = ORIENTED_EDGE ( 'NONE', *, *, #19759, .F. ) ;
#19962 = DIRECTION ( 'NONE',  ( 0.5000000000000051070, -0.8660254037844359321, 0.000000000000000000 ) ) ;
#19963 = CARTESIAN_POINT ( 'NONE',  ( 34.99529059433364608, 263.3427481158985302, 1.000000000000028644 ) ) ;
#19964 = CARTESIAN_POINT ( 'NONE',  ( 182.3972143829816730, 2.035126980567732780, -5.999999999999974243 ) ) ;
#19965 = CARTESIAN_POINT ( 'NONE',  ( 75.22395539455813207, 72.44174232321687157, -24.78378152481108643 ) ) ;
#19966 = CARTESIAN_POINT ( 'NONE',  ( -26.09897484109792742, 5.223491560547939727, 7.368033551913470092 ) ) ;
#19967 =( NAMED_UNIT ( * ) SI_UNIT ( $, .STERADIAN. ) SOLID_ANGLE_UNIT ( ) );
#19968 = DIRECTION ( 'NONE',  ( -1.000000000000000000, 0.000000000000000000, 0.000000000000000000 ) ) ;
#19969 = ORIENTED_EDGE ( 'NONE', *, *, #2145, .T. ) ;
#19970 = AXIS2_PLACEMENT_3D ( 'NONE', #16462, #4370, #7326 ) ;
#19971 = CARTESIAN_POINT ( 'NONE',  ( 82.36099222546647525, 65.03795902914596638, -25.63165455292080708 ) ) ;
#19972 = VECTOR ( 'NONE', #3307, 1000.000000000000114 ) ;
#19973 = CARTESIAN_POINT ( 'NONE',  ( 64.92628429094538944, 80.60227088397526529, -21.04771496906974448 ) ) ;
#19974 = EDGE_CURVE ( 'NONE', #13651, #2239, #10859, .T. ) ;
#19975 = AXIS2_PLACEMENT_3D ( 'NONE', #4056, #16788, #2267 ) ;
#19976 = ORIENTED_EDGE ( 'NONE', *, *, #14119, .F. ) ;
#19977 = ADVANCED_FACE ( 'NONE', ( #2 ), #6664, .T. ) ;
#19978 = CARTESIAN_POINT ( 'NONE',  ( 203.0966297564995671, 24.15688938925481111, -14.91618358615997408 ) ) ;
#19979 = CARTESIAN_POINT ( 'NONE',  ( -3.068708237237466108, 55.70095837538499950, -0.7135719611316724276 ) ) ;
#19980 = PLANE ( 'NONE',  #18067 ) ;
#19981 = B_SPLINE_CURVE_WITH_KNOTS ( 'NONE', 3,
 ( #13895, #12516, #2869, #854, #7304, #4140, #1281, #20241, #18772, #9415, #12830, #12721, #14747, #11024 ),
 .UNSPECIFIED., .F., .F.,
 ( 4, 2, 2, 2, 2, 2, 4 ),
 ( 1.510469127625910055E-17, 0.003820875137362821691, 0.005731312706044241860, 0.007641750274725663331, 0.01146262541208846811, 0.01337306298076985228, 0.01528350054945123472 ),
 .UNSPECIFIED. ) ;
#19982 = VECTOR ( 'NONE', #866, 1000.000000000000114 ) ;
#19983 = CARTESIAN_POINT ( 'NONE',  ( 105.7973891242897508, 30.70991617951901276, -12.50000000000000000 ) ) ;
#19984 = CARTESIAN_POINT ( 'NONE',  ( 97.64222899835127123, 199.2439717600714744, 9.012579768282821036 ) ) ;
#19985 = CARTESIAN_POINT ( 'NONE',  ( 229.7285650908456205, 36.81385593646026422, -13.56204498775466583 ) ) ;
#19987 = VERTEX_POINT ( 'NONE', #16323 ) ;
#19986 = ORIENTED_EDGE ( 'NONE', *, *, #1923, .F. ) ;
#19988 = ORIENTED_EDGE ( 'NONE', *, *, #19588, .T. ) ;
#19989 = CARTESIAN_POINT ( 'NONE',  ( 199.2144802262915846, 21.04890371929339921, -14.00000000000005507 ) ) ;
#19990 = B_SPLINE_CURVE_WITH_KNOTS ( 'NONE', 3,
 ( #8281, #12874, #6377, #9870 ),
 .UNSPECIFIED., .F., .F.,
 ( 4, 4 ),
 ( 5.481513501809308120E-07, 0.0006731989434038709343 ),
 .UNSPECIFIED. ) ;
#19991 = DIRECTION ( 'NONE',  ( -0.3430151393149036276, -0.1980398830195791438, 0.9182161068802751069 ) ) ;
#19992 = VECTOR ( 'NONE', #8479, 1000.000000000000114 ) ;
#19993 = AXIS2_PLACEMENT_3D ( 'NONE', #14939, #5566, #12059 ) ;
#19994 = ORIENTED_EDGE ( 'NONE', *, *, #343, .T. ) ;
#19995 = ORIENTED_EDGE ( 'NONE', *, *, #14220, .T. ) ;
#19996 = ORIENTED_EDGE ( 'NONE', *, *, #9891, .T. ) ;
#19997 = CARTESIAN_POINT ( 'NONE',  ( 81.20915916204526752, 64.82231599782905107, 0.5000000000000880407 ) ) ;
#19998 = CARTESIAN_POINT ( 'NONE',  ( 228.7990339483849596, 38.42385110241974644, -17.14987233279968848 ) ) ;
#19999 = CARTESIAN_POINT ( 'NONE',  ( 227.3013748640744893, 40.36491359635977005, -10.26496874235368040 ) ) ;
#20000 = VERTEX_POINT ( 'NONE', #15908 ) ;
#20001 = AXIS2_PLACEMENT_3D ( 'NONE', #14883, #5687, #6783 ) ;
#20002 = CARTESIAN_POINT ( 'NONE',  ( 30.00000000000000000, -10.00000000000000000, 28.99999999999999645 ) ) ;
#20003 = CARTESIAN_POINT ( 'NONE',  ( -18.56676705637232061, 70.73015596793582915, -4.299749073728317050 ) ) ;
#20004 = ADVANCED_FACE ( 'NONE', ( #19286 ), #6335, .T. ) ;
#20005 = ORIENTED_EDGE ( 'NONE', *, *, #7003, .F. ) ;
#20006 = CARTESIAN_POINT ( 'NONE',  ( 227.8089867185126991, 40.13866320645093566, -10.39224118001587449 ) ) ;
#20007 = EDGE_CURVE ( 'NONE', #12264, #11172, #19084, .T. ) ;
#20008 = VECTOR ( 'NONE', #3668, 1000.000000000000227 ) ;
#20009 = FACE_OUTER_BOUND ( 'NONE', #228, .T. ) ;
#20010 = CARTESIAN_POINT ( 'NONE',  ( -32.86183952535874653, 57.32352061648923325, 0.3918776291228620035 ) ) ;
#20011 = LINE ( 'NONE', #11859, #10939 ) ;
#20012 = AXIS2_PLACEMENT_3D ( 'NONE', #10725, #1512, #1305 ) ;
#20013 = VECTOR ( 'NONE', #2201, 1000.000000000000227 ) ;
#20014 = VERTEX_POINT ( 'NONE', #6434 ) ;
#20015 = EDGE_CURVE ( 'NONE', #4158, #6628, #11776, .T. ) ;
#20016 = CARTESIAN_POINT ( 'NONE',  ( 27.00000000000002487, 65.00000000000000000, -12.50000000000000000 ) ) ;
#20017 = VECTOR ( 'NONE', #18070, 999.9999999999998863 ) ;
#20018 = DIRECTION ( 'NONE',  ( -0.8660254037844357100, -0.5000000000000049960, 0.000000000000000000 ) ) ;
#20020 = ORIENTED_EDGE ( 'NONE', *, *, #18892, .F. ) ;
#20019 = VERTEX_POINT ( 'NONE', #1378 ) ;
#20021 = CARTESIAN_POINT ( 'NONE',  ( 56.75722135801910895, 76.93189375612146819, -17.66514001337803919 ) ) ;
#20022 = ORIENTED_EDGE ( 'NONE', *, *, #20067, .F. ) ;
#20023 = ORIENTED_EDGE ( 'NONE', *, *, #7606, .T. ) ;
#20024 = ADVANCED_FACE ( 'NONE', ( #12936 ), #9078, .F. ) ;
#20025 = VERTEX_POINT ( 'NONE', #17229 ) ;
#20026 = CARTESIAN_POINT ( 'NONE',  ( 34.99529059433359635, 263.3427481158985870, -5.999999999999973355 ) ) ;
#20027 = CARTESIAN_POINT ( 'NONE',  ( 203.5544658059540666, 23.53182819120163671, -14.00000000000005507 ) ) ;
#20028 = VECTOR ( 'NONE', #5222, 1000.000000000000000 ) ;
#20029 = ORIENTED_EDGE ( 'NONE', *, *, #16529, .T. ) ;
#20030 = FACE_OUTER_BOUND ( 'NONE', #8275, .T. ) ;
#20031 = EDGE_LOOP ( 'NONE', ( #11666, #9908, #9909, #19389, #2948 ) ) ;
#20032 = ADVANCED_FACE ( 'NONE', ( #18720 ), #17124, .F. ) ;
#20033 = CARTESIAN_POINT ( 'NONE',  ( 221.0233832323356751, 33.37515478688916915, -16.82415462623112390 ) ) ;
#20034 = AXIS2_PLACEMENT_3D ( 'NONE', #18800, #18910, #4173 ) ;
#20035 = FACE_OUTER_BOUND ( 'NONE', #8815, .T. ) ;
#20036 = DIRECTION ( 'NONE',  ( 0.8660254037844372643, 0.5000000000000027756, -0.000000000000000000 ) ) ;
#20037 = DIRECTION ( 'NONE',  ( 1.000000000000000000, 0.000000000000000000, 0.000000000000000000 ) ) ;
#20038 = LINE ( 'NONE', #3605, #19158 ) ;
#20039 = LINE ( 'NONE', #18452, #16345 ) ;
#20040 = EDGE_CURVE ( 'NONE', #4395, #14638, #5658, .T. ) ;
#20041 = CARTESIAN_POINT ( 'NONE',  ( 227.1431551712864803, 41.29191727552926494, -10.76535568099441420 ) ) ;
#20042 = COLOUR_RGB ( '',0.7921568627450980005, 0.8196078431372548767, 0.9333333333333333481 ) ;
#20043 = PLANE ( 'NONE',  #13687 ) ;
#20044 = CARTESIAN_POINT ( 'NONE',  ( 226.9304947408143391, 41.66025594586614034, -16.98332657222546871 ) ) ;
#20045 = ORIENTED_EDGE ( 'NONE', *, *, #8707, .F. ) ;
#20046 = VECTOR ( 'NONE', #20560, 999.9999999999998863 ) ;
#20047 = AXIS2_PLACEMENT_3D ( 'NONE', #9356, #904, #4507 ) ;
#20048 = DIRECTION ( 'NONE',  ( -0.6946590618905411629, -0.4010615963775225890, 0.5971585917027958379 ) ) ;
#20049 = ADVANCED_FACE ( 'NONE', ( #20092 ), #14062, .T. ) ;
#20050 = EDGE_CURVE ( 'NONE', #9060, #2720, #7464, .T. ) ;
#20051 = EDGE_LOOP ( 'NONE', ( #19142, #12974, #2440, #10485, #1646 ) ) ;
#20052 = FACE_OUTER_BOUND ( 'NONE', #5164, .T. ) ;
#20053 = CARTESIAN_POINT ( 'NONE',  ( 205.5965122587965084, 9.994899983462953941, -14.00000000000005507 ) ) ;
#20054 = EDGE_LOOP ( 'NONE', ( #852, #19404, #14677, #12218 ) ) ;
#20055 = ADVANCED_FACE ( 'NONE', ( #18822 ), #10641, .T. ) ;
#20056 = APPLICATION_PROTOCOL_DEFINITION ( 'draft international standard', 'automotive_design', 1998, #927 ) ;
#20057 = ADVANCED_FACE ( 'NONE', ( #5976 ), #8951, .F. ) ;
#20058 = FACE_OUTER_BOUND ( 'NONE', #5346, .T. ) ;
#20059 = VERTEX_POINT ( 'NONE', #12468 ) ;
#20060 = CARTESIAN_POINT ( 'NONE',  ( 81.27728676539042851, 64.71885472535731765, -25.49785049058046837 ) ) ;
#20061 = CARTESIAN_POINT ( 'NONE',  ( 226.6211368133091923, 39.11482588413117867, -14.00000000000005507 ) ) ;
#20062 = CONICAL_SURFACE ( 'NONE', #2126, 10.85470691220533190, 0.8171114040043576665 ) ;
#20063 = CARTESIAN_POINT ( 'NONE',  ( 226.7034097767528067, 42.05357864125575418, -16.61383192937491771 ) ) ;
#20064 = CARTESIAN_POINT ( 'NONE',  ( 213.2500461588270468, 13.88262057910513825, -23.06309126349817618 ) ) ;
#20065 = ORIENTED_EDGE ( 'NONE', *, *, #3566, .F. ) ;
#20066 = DIRECTION ( 'NONE',  ( -0.5000000000000046629, 0.8660254037844359321, 0.000000000000000000 ) ) ;
#20067 = EDGE_CURVE ( 'NONE', #10601, #12839, #2476, .T. ) ;
#20068 = DIRECTION ( 'NONE',  ( -1.000000000000000000, 0.000000000000000000, -0.000000000000000000 ) ) ;
#20069 = DIRECTION ( 'NONE',  ( 0.8660254037844375974, 0.5000000000000019984, -4.996003610813205418E-16 ) ) ;
#20070 = VERTEX_POINT ( 'NONE', #20402 ) ;
#20071 = CARTESIAN_POINT ( 'NONE',  ( 84.01452848080124625, 118.4389375482329001, -29.00000000000002487 ) ) ;
#20072 = LINE ( 'NONE', #8518, #14629 ) ;
#20073 = CARTESIAN_POINT ( 'NONE',  ( -15.99999999999999289, 79.99999999999998579, -12.50000000000000000 ) ) ;
#20074 = VECTOR ( 'NONE', #18214, 1000.000000000000000 ) ;
#20076 = ORIENTED_EDGE ( 'NONE', *, *, #16615, .F. ) ;
#20075 = ORIENTED_EDGE ( 'NONE', *, *, #14998, .F. ) ;
#20077 = ORIENTED_EDGE ( 'NONE', *, *, #6384, .F. ) ;
#20078 = DIRECTION ( 'NONE',  ( 0.000000000000000000, 1.000000000000000000, 0.000000000000000000 ) ) ;
#20079 = DIRECTION ( 'NONE',  ( 0.000000000000000000, -0.5000000000000009992, -0.8660254037844380415 ) ) ;
#20080 = CARTESIAN_POINT ( 'NONE',  ( -32.42127702560121350, 78.26431280098985610, -5.492938746012961282 ) ) ;
#20081 = CARTESIAN_POINT ( 'NONE',  ( 80.27267528958725507, 52.02232914097061212, -19.70798756841603350 ) ) ;
#20082 = EDGE_CURVE ( 'NONE', #2368, #425, #15351, .T. ) ;
#20083 = CARTESIAN_POINT ( 'NONE',  ( -26.92417954832534122, 9.835141389658375033, 6.084915548678262454 ) ) ;
#20084 =( LENGTH_UNIT ( ) NAMED_UNIT ( * ) SI_UNIT ( .MILLI., .METRE. ) );
#20085 = DIRECTION ( 'NONE',  ( -0.9367698044638429478, 0.000000000000000000, -0.3499461864984006465 ) ) ;
#20086 = ORIENTED_EDGE ( 'NONE', *, *, #15850, .T. ) ;
#20087 = CARTESIAN_POINT ( 'NONE',  ( 82.87350344862416307, 63.33930485192262694, -25.52864195477530984 ) ) ;
#20088 = FACE_OUTER_BOUND ( 'NONE', #12625, .T. ) ;
#20089 = AXIS2_PLACEMENT_3D ( 'NONE', #5138, #11626, #16397 ) ;
#20090 = VERTEX_POINT ( 'NONE', #20498 ) ;
#20091 = CARTESIAN_POINT ( 'NONE',  ( 202.9101512355597094, 24.36019071069245356, -15.19895601951926878 ) ) ;
#20092 = FACE_OUTER_BOUND ( 'NONE', #14399, .T. ) ;
#20093 = DIRECTION ( 'NONE',  ( 0.000000000000000000, 0.000000000000000000, -1.000000000000000000 ) ) ;
#20094 = DIRECTION ( 'NONE',  ( -0.5000000000000054401, 0.8660254037844354880, -0.000000000000000000 ) ) ;
#20095 = EDGE_CURVE ( 'NONE', #20283, #5044, #20294, .T. ) ;
#20096 = LINE ( 'NONE', #20299, #17833 ) ;
#20098 = ORIENTED_EDGE ( 'NONE', *, *, #20410, .T. ) ;
#20097 = ORIENTED_EDGE ( 'NONE', *, *, #11199, .T. ) ;
#20099 = VERTEX_POINT ( 'NONE', #909 ) ;
#20100 = CARTESIAN_POINT ( 'NONE',  ( 221.7323030100353662, 32.17036527648973276, -14.00000000000005507 ) ) ;
#20101 = DIRECTION ( 'NONE',  ( 0.5000000000000015543, -0.8660254037844377084, 0.000000000000000000 ) ) ;
#20102 = ORIENTED_EDGE ( 'NONE', *, *, #14323, .T. ) ;
#20103 = VERTEX_POINT ( 'NONE', #3869 ) ;
#20104 = CARTESIAN_POINT ( 'NONE',  ( 0.000000000000000000, 2.342598717236913153, 4.057499999999995666 ) ) ;
#20105 = DIRECTION ( 'NONE',  ( 0.000000000000000000, 0.7775157341892985352, -0.6288634852558033783 ) ) ;
#20106 = DIRECTION ( 'NONE',  ( -0.5016613886297335290, 0.000000000000000000, -0.8650640734408565624 ) ) ;
#20107 = CIRCLE ( 'NONE', #20764, 0.4000000000000001887 ) ;
#20108 = VECTOR ( 'NONE', #17499, 1000.000000000000227 ) ;
#20109 = ORIENTED_EDGE ( 'NONE', *, *, #14882, .T. ) ;
#20110 = PLANE ( 'NONE',  #6596 ) ;
#20111 = EDGE_CURVE ( 'NONE', #2861, #2041, #18450, .T. ) ;
#20112 = CARTESIAN_POINT ( 'NONE',  ( 221.7170026686113147, 32.20379548820332616, -14.53509620734056540 ) ) ;
#20113 = EDGE_LOOP ( 'NONE', ( #2732, #10703, #8274, #10147 ) ) ;
#20114 = DIRECTION ( 'NONE',  ( -0.8660254037844373753, -0.5000000000000022204, 0.000000000000000000 ) ) ;
#20115 = FACE_OUTER_BOUND ( 'NONE', #17555, .T. ) ;
#20116 = CARTESIAN_POINT ( 'NONE',  ( -24.74740475360116321, 50.13270831063489652, -14.49843712002114238 ) ) ;
#20117 = CARTESIAN_POINT ( 'NONE',  ( 228.4171206443014910, 38.10587845811534180, -10.52303454827241502 ) ) ;
#20118 = DIRECTION ( 'NONE',  ( -1.000000000000000000, 0.000000000000000000, 0.000000000000000000 ) ) ;
#20119 = CARTESIAN_POINT ( 'NONE',  ( -27.82037292730693778, 56.67161465046595481, 4.072047940184197579 ) ) ;
#20121 = ORIENTED_EDGE ( 'NONE', *, *, #1645, .T. ) ;
#20120 = ORIENTED_EDGE ( 'NONE', *, *, #20369, .F. ) ;
#20122 = CARTESIAN_POINT ( 'NONE',  ( 60.93143657513353872, 83.68840998819324284, -17.92058816135999422 ) ) ;
#20123 = ORIENTED_EDGE ( 'NONE', *, *, #18046, .F. ) ;
#20124 = VERTEX_POINT ( 'NONE', #13639 ) ;
#20125 = ORIENTED_EDGE ( 'NONE', *, *, #20256, .F. ) ;
#20126 = CARTESIAN_POINT ( 'NONE',  ( 218.5440333250598997, 38.31738797143729869, -16.00491213559310921 ) ) ;
#20127 = DIRECTION ( 'NONE',  ( -0.8944271909999204073, 0.000000000000000000, -0.4472135954999487684 ) ) ;
#20128 = EDGE_CURVE ( 'NONE', #9755, #9039, #14505, .T. ) ;
#20129 = VERTEX_POINT ( 'NONE', #7355 ) ;
#20130 = ORIENTED_EDGE ( 'NONE', *, *, #5233, .F. ) ;
#20131 = EDGE_CURVE ( 'NONE', #16536, #20133, #10429, .T. ) ;
#20132 = CARTESIAN_POINT ( 'NONE',  ( 219.4414768585382944, 34.63161541676048927, -9.756613004592562532 ) ) ;
#20133 = VERTEX_POINT ( 'NONE', #7256 ) ;
#20134 = VECTOR ( 'NONE', #8843, 1000.000000000000114 ) ;
#20135 = DIRECTION ( 'NONE',  ( -0.8660254037844355990, -0.5000000000000055511, 0.000000000000000000 ) ) ;
#20136 = CYLINDRICAL_SURFACE ( 'NONE', #801, 9.999999999999998224 ) ;
#20137 = CARTESIAN_POINT ( 'NONE',  ( -15.99999999999999289, 20.09941697557067997, 12.50000000000000000 ) ) ;
#20138 = EDGE_CURVE ( 'NONE', #13568, #4595, #8606, .T. ) ;
#20139 = VERTEX_POINT ( 'NONE', #12147 ) ;
#20140 = CARTESIAN_POINT ( 'NONE',  ( 34.99529059433364608, 263.3427481158985302, -28.99999999999997513 ) ) ;
#20141 = CARTESIAN_POINT ( 'NONE',  ( 214.9714796170919442, 8.242131668836057301, -23.72013913782489425 ) ) ;
#20142 = CYLINDRICAL_SURFACE ( 'NONE', #17025, 5.000000000000008882 ) ;
#20143 = CARTESIAN_POINT ( 'NONE',  ( -33.06477925144887564, 73.59974835485031974, -0.1995438761935474647 ) ) ;
#20144 = CYLINDRICAL_SURFACE ( 'NONE', #3175, 12.47473710546057646 ) ;
#20145 = DIRECTION ( 'NONE',  ( 0.000000000000000000, 0.5134338004640686126, -0.8581292050390914028 ) ) ;
#20146 = ORIENTED_EDGE ( 'NONE', *, *, #4972, .T. ) ;
#20148 = EDGE_CURVE ( 'NONE', #17008, #14920, #592, .T. ) ;
#20147 = CARTESIAN_POINT ( 'NONE',  ( -3.241054845510801918, 65.75000000000000000, 3.522626389267836444 ) ) ;
#20149 = AXIS2_PLACEMENT_3D ( 'NONE', #19710, #16752, #439 ) ;
#20150 = ORIENTED_EDGE ( 'NONE', *, *, #13923, .T. ) ;
#20151 = CARTESIAN_POINT ( 'NONE',  ( -11.00000000000000355, 15.09941697557068530, 15.00000000000000000 ) ) ;
#20152 = CARTESIAN_POINT ( 'NONE',  ( 184.9952905943349606, 3.535126980567727450, -29.00000000000001066 ) ) ;
#20153 = EDGE_CURVE ( 'NONE', #4182, #12636, #13461, .T. ) ;
#20154 = CARTESIAN_POINT ( 'NONE',  ( 221.5905601460494552, 32.21316951758458913, -14.00000000000005507 ) ) ;
#20155 = ORIENTED_EDGE ( 'NONE', *, *, #12815, .F. ) ;
#20156 = CARTESIAN_POINT ( 'NONE',  ( 81.45283486207161161, 64.41465532991168175, -25.48770694380405288 ) ) ;
#20157 = CLOSED_SHELL ( 'NONE', ( #12015, #3806, #15870, #729, #16260, #14348, #15779, #2801, #16618, #17052, #15076, #1273, #5468, #14991, #2478, #13535, #9922, #15767, #11739, #13650, #9464, #18581, #2207, #14612, #6535, #6177, #13593 ) ) ;
#20158 = FACE_OUTER_BOUND ( 'NONE', #8577, .T. ) ;
#20159 = CARTESIAN_POINT ( 'NONE',  ( 89.99529059433416478, 168.0799536996104848, 26.00000000000001066 ) ) ;
#20160 = FACE_OUTER_BOUND ( 'NONE', #4047, .T. ) ;
#20161 = EDGE_CURVE ( 'NONE', #6893, #2640, #16690, .T. ) ;
#20162 = EDGE_CURVE ( 'NONE', #13052, #14788, #6076, .T. ) ;
#20163 = CIRCLE ( 'NONE', #6960, 12.47473710546057823 ) ;
#20164 = DIRECTION ( 'NONE',  ( -0.8660254037844355990, -0.5000000000000053291, 0.000000000000000000 ) ) ;
#20165 = AXIS2_PLACEMENT_3D ( 'NONE', #3976, #20686, #17021 ) ;
#20166 = CARTESIAN_POINT ( 'NONE',  ( 226.6218208878421194, 41.21542885111893639, -17.45257705044830843 ) ) ;
#20167 = DIRECTION ( 'NONE',  ( -1.000000000000000000, 0.000000000000000000, 0.000000000000000000 ) ) ;
#20168 = ORIENTED_EDGE ( 'NONE', *, *, #3595, .T. ) ;
#20170 = EDGE_CURVE ( 'NONE', #11314, #11315, #7693, .T. ) ;
#20169 = DIRECTION ( 'NONE',  ( 0.000000000000000000, 0.000000000000000000, 1.000000000000000000 ) ) ;
#20171 = CARTESIAN_POINT ( 'NONE',  ( 177.1791022559528983, 56.75747545832872731, -14.00000000000006395 ) ) ;
#20172 = AXIS2_PLACEMENT_3D ( 'NONE', #1757, #17562, #19545 ) ;
#20173 = DIRECTION ( 'NONE',  ( 0.000000000000000000, -0.000000000000000000, -1.000000000000000000 ) ) ;
#20174 = CARTESIAN_POINT ( 'NONE',  ( -15.73951528932505894, 79.99999999999998579, -12.50000000001717204 ) ) ;
#20176 = VERTEX_POINT ( 'NONE', #4399 ) ;
#20175 = ORIENTED_EDGE ( 'NONE', *, *, #1526, .T. ) ;
#20177 = ORIENTED_EDGE ( 'NONE', *, *, #1517, .F. ) ;
#20178 = DIRECTION ( 'NONE',  ( 0.5000000000000053291, -0.8660254037844355990, -2.220446049250312588E-16 ) ) ;
#20179 = FILL_AREA_STYLE ('',( #15646 ) ) ;
#20180 = VECTOR ( 'NONE', #5796, 1000.000000000000000 ) ;
#20181 = ORIENTED_EDGE ( 'NONE', *, *, #2414, .F. ) ;
#20182 = CARTESIAN_POINT ( 'NONE',  ( 228.0559782506801980, 39.71086132369779165, -17.61401795338991505 ) ) ;
#20183 = ADVANCED_FACE ( 'NONE', ( #17757 ), #7883, .F. ) ;
#20184 = CARTESIAN_POINT ( 'NONE',  ( 196.4465031000483179, 4.712139732572081741, -8.669480444820576892 ) ) ;
#20185 = CARTESIAN_POINT ( 'NONE',  ( -30.00000000000032330, 4.999999999999686473, 1.877804259809431997 ) ) ;
#20186 =( NAMED_UNIT ( * ) SI_UNIT ( $, .STERADIAN. ) SOLID_ANGLE_UNIT ( ) );
#20187 = DIRECTION ( 'NONE',  ( 0.5000000000000041078, -0.8660254037844361541, 0.000000000000000000 ) ) ;
#20188 = ORIENTED_EDGE ( 'NONE', *, *, #39, .T. ) ;
#20189 = CARTESIAN_POINT ( 'NONE',  ( 81.30519808514482349, 55.03237058933864034, -22.52907132704141802 ) ) ;
#20190 = AXIS2_PLACEMENT_3D ( 'NONE', #2607, #18810, #17219 ) ;
#20191 = CARTESIAN_POINT ( 'NONE',  ( 217.8425870996167077, 37.40097371491418698, -17.10689588174065179 ) ) ;
#20192 = ORIENTED_EDGE ( 'NONE', *, *, #1246, .F. ) ;
#20193 = VECTOR ( 'NONE', #4621, 1000.000000000000000 ) ;
#20194 = PLANE ( 'NONE',  #4770 ) ;
#20195 = FACE_OUTER_BOUND ( 'NONE', #11999, .T. ) ;
#20196 = DIRECTION ( 'NONE',  ( 0.8660254037844355990, 0.5000000000000054401, 3.615531934188343626E-15 ) ) ;
#20197 = CARTESIAN_POINT ( 'NONE',  ( 218.2235991490363745, 38.25454787544715174, -14.91677899116112016 ) ) ;
#20198 = EDGE_LOOP ( 'NONE', ( #7913, #19053, #16632, #2776, #16131, #3316, #5171, #18885, #19525, #7887, #8826 ) ) ;
#20199 = EDGE_LOOP ( 'NONE', ( #16532, #1805, #5373, #7364 ) ) ;
#20200 = CARTESIAN_POINT ( 'NONE',  ( 221.5989882111056772, 32.37817771857039162, -15.28456752314060552 ) ) ;
#20201 = DIRECTION ( 'NONE',  ( -0.8660254037844378194, -0.5000000000000013323, -0.000000000000000000 ) ) ;
#20202 = ORIENTED_EDGE ( 'NONE', *, *, #11032, .T. ) ;
#20203 = ORIENTED_EDGE ( 'NONE', *, *, #10117, .F. ) ;
#20204 = CARTESIAN_POINT ( 'NONE',  ( 196.1661066256804986, 4.019203490823548997, -8.415281845791808379 ) ) ;
#20205 = CARTESIAN_POINT ( 'NONE',  ( 31.00000000000000711, 65.00000000000000000, -12.50000000000000000 ) ) ;
#20206 = DIRECTION ( 'NONE',  ( 0.8660254037844372643, 0.5000000000000027756, -0.000000000000000000 ) ) ;
#20207 = ORIENTED_EDGE ( 'NONE', *, *, #10809, .T. ) ;
#20208 = AXIS2_PLACEMENT_3D ( 'NONE', #3859, #18278, #15024 ) ;
#20209 = CARTESIAN_POINT ( 'NONE',  ( 208.9378540577313004, 11.39297530874010000, -25.94618751764496878 ) ) ;
#20210 = VERTEX_POINT ( 'NONE', #15761 ) ;
#20211 = CARTESIAN_POINT ( 'NONE',  ( 59.39721438298058587, 215.0773763115390125, -22.00000000000000355 ) ) ;
#20212 = CYLINDRICAL_SURFACE ( 'NONE', #18025, 4.999999999999990230 ) ;
#20213 = CARTESIAN_POINT ( 'NONE',  ( -13.59909031749119102, 50.44595023350106544, -16.13088894857765965 ) ) ;
#20214 = CARTESIAN_POINT ( 'NONE',  ( 182.5734976231970563, 59.87193107572243633, -14.00000000000002842 ) ) ;
#20215 = DIRECTION ( 'NONE',  ( 0.8660254037844355990, 0.5000000000000054401, -1.334965637238773043E-14 ) ) ;
#20216 = LINE ( 'NONE', #5684, #1560 ) ;
#20217 = VECTOR ( 'NONE', #721, 1000.000000000000114 ) ;
#20218 = EDGE_CURVE ( 'NONE', #8882, #8243, #12148, .T. ) ;
#20220 = ORIENTED_EDGE ( 'NONE', *, *, #82, .T. ) ;
#20219 = ORIENTED_EDGE ( 'NONE', *, *, #5465, .T. ) ;
#20221 = CARTESIAN_POINT ( 'NONE',  ( 198.8331280799749550, -1.075349935395403689, -9.858802615641089062 ) ) ;
#20222 = CARTESIAN_POINT ( 'NONE',  ( 63.81044076472581850, 77.45544899285202689, -17.65926648166063373 ) ) ;
#20223 = AXIS2_PLACEMENT_3D ( 'NONE', #2920, #7985, #3126 ) ;
#20224 = ORIENTED_EDGE ( 'NONE', *, *, #16761, .F. ) ;
#20225 = ORIENTED_EDGE ( 'NONE', *, *, #8634, .T. ) ;
#20226 = ORIENTED_EDGE ( 'NONE', *, *, #12890, .F. ) ;
#20227 = CARTESIAN_POINT ( 'NONE',  ( 95.83809698076872507, 24.95991617951895236, -12.50000000000000000 ) ) ;
#20228 = LINE ( 'NONE', #5807, #2924 ) ;
#20229 = ORIENTED_EDGE ( 'NONE', *, *, #17823, .T. ) ;
#20230 = VERTEX_POINT ( 'NONE', #16171 ) ;
#20231 = CARTESIAN_POINT ( 'NONE',  ( 35.35427444295658006, 182.7209698509878422, 11.00000000000001243 ) ) ;
#20232 = B_SPLINE_CURVE_WITH_KNOTS ( 'NONE', 3,
 ( #2484, #10952, #14152, #2899, #993, #12449, #15428, #7758, #4171, #14042, #14261, #5849, #15537, #7437 ),
 .UNSPECIFIED., .F., .F.,
 ( 4, 2, 2, 2, 2, 2, 4 ),
 ( 0.000000000000000000, 0.001925163319758125494, 0.003850326639516250989, 0.007700653279032461211, 0.009625816598790543771, 0.01155097991854863067, 0.01540130655806476456 ),
 .UNSPECIFIED. ) ;
#20234 = EDGE_CURVE ( 'NONE', #9307, #6007, #7778, .T. ) ;
#20233 = CARTESIAN_POINT ( 'NONE',  ( 230.0035647074226972, 36.33754262848680128, -15.14518239232902275 ) ) ;
#20235 = DIRECTION ( 'NONE',  ( -1.000000000000000000, -0.000000000000000000, -0.000000000000000000 ) ) ;
#20236 = CIRCLE ( 'NONE', #1620, 3.902363844300875240 ) ;
#20237 = PRODUCT ( 'Drill Bit Assembly Sliding Track Base', 'Drill Bit Assembly Sliding Track Base', '', ( #19198 ) ) ;
#20238 = CARTESIAN_POINT ( 'NONE',  ( 199.2144802262915846, 21.04890371929339921, -14.00000000000005507 ) ) ;
#20239 = VECTOR ( 'NONE', #17489, 1000.000000000000114 ) ;
#20240 = LINE ( 'NONE', #5819, #3111 ) ;
#20241 = CARTESIAN_POINT ( 'NONE',  ( -27.68173125899994602, 72.07281518094384865, 4.467622400254045445 ) ) ;
#20242 = DIRECTION ( 'NONE',  ( 0.8660254037844360431, 0.5000000000000045519, 0.000000000000000000 ) ) ;
#20243 = EDGE_CURVE ( 'NONE', #15175, #6192, #1639, .T. ) ;
#20244 = ORIENTED_EDGE ( 'NONE', *, *, #17701, .F. ) ;
#20245 = CARTESIAN_POINT ( 'NONE',  ( -32.82806271630868622, 72.52289824211611347, 0.4796438872512392426 ) ) ;
#20246 = FACE_OUTER_BOUND ( 'NONE', #3670, .T. ) ;
#20247 = LINE ( 'NONE', #15304, #20710 ) ;
#20248 = EDGE_CURVE ( 'NONE', #8157, #15901, #11091, .T. ) ;
#20249 = ORIENTED_EDGE ( 'NONE', *, *, #665, .F. ) ;
#20250 = CARTESIAN_POINT ( 'NONE',  ( -0.6518013096703926257, 65.74999999999997158, 2.481238266578629226 ) ) ;
#20251 = AXIS2_PLACEMENT_3D ( 'NONE', #20877, #17618, #7950 ) ;
#20252 = ORIENTED_EDGE ( 'NONE', *, *, #7902, .F. ) ;
#20253 = CARTESIAN_POINT ( 'NONE',  ( 199.2144802262915846, 21.04890371929339921, -14.00000000000005507 ) ) ;
#20254 = LINE ( 'NONE', #3936, #4255 ) ;
#20255 = AXIS2_PLACEMENT_3D ( 'NONE', #20364, #8916, #13911 ) ;
#20256 = EDGE_CURVE ( 'NONE', #3900, #1433, #1226, .T. ) ;
#20257 = APPLICATION_PROTOCOL_DEFINITION ( 'draft international standard', 'automotive_design', 1998, #18665 ) ;
#20258 = CARTESIAN_POINT ( 'NONE',  ( 206.4249228987308413, 10.47318308942859133, -14.95831141195905190 ) ) ;
#20259 = ORIENTED_EDGE ( 'NONE', *, *, #171, .F. ) ;
#20260 = DIRECTION ( 'NONE',  ( 1.000000000000000000, 0.000000000000000000, 0.000000000000000000 ) ) ;
#20261 = DIRECTION ( 'NONE',  ( -0.4999999999999995004, 0.8660254037844390407, 0.000000000000000000 ) ) ;
#20262 = CARTESIAN_POINT ( 'NONE',  ( 31.00000000000000711, 75.00000000000000000, -12.50000000000000000 ) ) ;
#20263 = CARTESIAN_POINT ( 'NONE',  ( 229.9065197826579094, 36.50562936879610021, -12.30768923015400418 ) ) ;
#20264 = EDGE_CURVE ( 'NONE', #14662, #5690, #52, .T. ) ;
#20265 = AXIS2_PLACEMENT_3D ( 'NONE', #19, #4979, #19500 ) ;
#20266 = LINE ( 'NONE', #15630, #6161 ) ;
#20267 = ADVANCED_FACE ( 'NONE', ( #6490 ), #7007, .T. ) ;
#20268 = LINE ( 'NONE', #3952, #6841 ) ;
#20269 = CARTESIAN_POINT ( 'NONE',  ( -28.23156009437249025, 64.24999999999998579, 3.993547312438774366 ) ) ;
#20270 = VERTEX_POINT ( 'NONE', #10858 ) ;
#20271 = DIRECTION ( 'NONE',  ( 0.3654179821390644567, -0.6329225110641519825, -0.6825531432186526803 ) ) ;
#20272 = CARTESIAN_POINT ( 'NONE',  ( -29.99999999999999645, 5.000000000000000000, 15.00000000000000000 ) ) ;
#20273 = CARTESIAN_POINT ( 'NONE',  ( 30.10683012259193703, 5.000000000000000000, 4.999999999999997335 ) ) ;
#20274 = DIRECTION ( 'NONE',  ( -0.4084849465052216022, 0.7075166814740940779, -0.5766803221148710801 ) ) ;
#20275 = ADVANCED_FACE ( 'NONE', ( #2820 ), #15857, .T. ) ;
#20277 = ORIENTED_EDGE ( 'NONE', *, *, #4890, .F. ) ;
#20276 = ORIENTED_EDGE ( 'NONE', *, *, #2618, .F. ) ;
#20278 = ORIENTED_EDGE ( 'NONE', *, *, #6158, .T. ) ;
#20279 = EDGE_CURVE ( 'NONE', #9425, #14614, #13657, .T. ) ;
#20280 = VECTOR ( 'NONE', #19182, 1000.000000000000000 ) ;
#20281 = FACE_OUTER_BOUND ( 'NONE', #19467, .T. ) ;
#20282 = CARTESIAN_POINT ( 'NONE',  ( 229.6037303676573629, 37.03007601957109074, -12.62147488791610961 ) ) ;
#20283 = VERTEX_POINT ( 'NONE', #19241 ) ;
#20284 = CARTESIAN_POINT ( 'NONE',  ( -27.63293763622268528, 79.71668407523966948, -9.567129279037617451 ) ) ;
#20285 = CARTESIAN_POINT ( 'NONE',  ( 197.5001239273001659, -2.102559465580161380, -12.41782726985249319 ) ) ;
#20286 = DIRECTION ( 'NONE',  ( 0.5000000000000054401, -0.8660254037844354880, 0.000000000000000000 ) ) ;
#20287 = EDGE_CURVE ( 'NONE', #18356, #16672, #4608, .T. ) ;
#20288 = ORIENTED_EDGE ( 'NONE', *, *, #8441, .T. ) ;
#20289 = CARTESIAN_POINT ( 'NONE',  ( 198.2043721129365395, -1.441146303136960682, -13.99491531967994007 ) ) ;
#20290 = CARTESIAN_POINT ( 'NONE',  ( 229.0176887497488849, 38.04512987713822270, -11.06956603356930202 ) ) ;
#20291 = AXIS2_PLACEMENT_3D ( 'NONE', #2632, #10660, #2733 ) ;
#20292 = ORIENTED_EDGE ( 'NONE', *, *, #19702, .T. ) ;
#20293 = PLANE ( 'NONE',  #19649 ) ;
#20294 = LINE ( 'NONE', #15243, #8029 ) ;
#20295 = AXIS2_PLACEMENT_3D ( 'NONE', #11180, #19038, #4513 ) ;
#20296 = ADVANCED_FACE ( 'NONE', ( #11178 ), #4814, .F. ) ;
#20297 = CARTESIAN_POINT ( 'NONE',  ( 8.399999999999998579, 4.898587196589412829E-16, -4.000000000000000000 ) ) ;
#20298 = FACE_BOUND ( 'NONE', #2604, .T. ) ;
#20299 = CARTESIAN_POINT ( 'NONE',  ( 85.37797649651368204, 230.0773763115391262, 1.000000000000017097 ) ) ;
#20300 = CIRCLE ( 'NONE', #7429, 12.00000000000000178 ) ;
#20301 = ORIENTED_EDGE ( 'NONE', *, *, #20692, .F. ) ;
#20302 = ORIENTED_EDGE ( 'NONE', *, *, #15677, .F. ) ;
#20303 = DIRECTION ( 'NONE',  ( -0.5000000000000045519, 0.8660254037844361541, 0.000000000000000000 ) ) ;
#20304 = DIRECTION ( 'NONE',  ( 1.000000000000000000, -0.000000000000000000, -0.000000000000000000 ) ) ;
#20305 = VECTOR ( 'NONE', #13803, 1000.000000000000227 ) ;
#20306 = EDGE_CURVE ( 'NONE', #18834, #8493, #16513, .T. ) ;
#20307 = ORIENTED_EDGE ( 'NONE', *, *, #13828, .F. ) ;
#20308 = EDGE_LOOP ( 'NONE', ( #13745, #5926, #1722, #8041, #11465, #18241 ) ) ;
#20309 = EDGE_CURVE ( 'NONE', #2193, #6975, #8513, .T. ) ;
#20310 = CARTESIAN_POINT ( 'NONE',  ( 220.4979741297062219, 34.72708515683768837, -10.27986985910186135 ) ) ;
#20311 = DIRECTION ( 'NONE',  ( 0.000000000000000000, 0.000000000000000000, 1.000000000000000000 ) ) ;
#20312 = CYLINDRICAL_SURFACE ( 'NONE', #4955, 4.999999999999989342 ) ;
#20313 = DIRECTION ( 'NONE',  ( -0.8660254037844350439, -0.5000000000000061062, 0.000000000000000000 ) ) ;
#20314 = CARTESIAN_POINT ( 'NONE',  ( 218.7131701895986851, 37.40658595927892094, -16.57782486433068669 ) ) ;
#20315 = VERTEX_POINT ( 'NONE', #13091 ) ;
#20316 = AXIS2_PLACEMENT_3D ( 'NONE', #14802, #12992, #13095 ) ;
#20317 = DIRECTION ( 'NONE',  ( -0.000000000000000000, -1.000000000000000000, -0.000000000000000000 ) ) ;
#20318 = AXIS2_PLACEMENT_3D ( 'NONE', #10710, #2248, #4036 ) ;
#20319 = CARTESIAN_POINT ( 'NONE',  ( 213.9169459704606879, 7.890903399153988751, -24.64792178047109417 ) ) ;
#20320 = CARTESIAN_POINT ( 'NONE',  ( -23.12579181598519540, 45.08735423564900913, -10.27585172372141287 ) ) ;
#20321 = CARTESIAN_POINT ( 'NONE',  ( 228.7675624436089095, 38.47836134768217420, -10.76535568099436446 ) ) ;
#20322 = CIRCLE ( 'NONE', #8131, 2.499999999999997780 ) ;
#20323 = DIRECTION ( 'NONE',  ( -0.08515265670862154357, 0.1474887278187986539, 0.9853913436913560586 ) ) ;
#20324 = CARTESIAN_POINT ( 'NONE',  ( -28.34202942068278475, 47.50017047936148629, -2.003691985157042055 ) ) ;
#20326 = ORIENTED_EDGE ( 'NONE', *, *, #16130, .T. ) ;
#20325 = ORIENTED_EDGE ( 'NONE', *, *, #8874, .T. ) ;
#20327 = CIRCLE ( 'NONE', #13912, 3.619616396367202782 ) ;
#20328 = CARTESIAN_POINT ( 'NONE',  ( 201.9232776496033637, 26.15921614160104980, -13.00767012778560705 ) ) ;
#20329 = DIRECTION ( 'NONE',  ( 0.5000000000000049960, -0.8660254037844358210, 0.000000000000000000 ) ) ;
#20330 = FACE_OUTER_BOUND ( 'NONE', #5685, .T. ) ;
#20331 = CIRCLE ( 'NONE', #10855, 7.155882939242646401 ) ;
#20332 = ORIENTED_EDGE ( 'NONE', *, *, #118, .F. ) ;
#20333 = CARTESIAN_POINT ( 'NONE',  ( 218.5975169673276355, 10.59323232415630756, -18.20125362229464372 ) ) ;
#20334 = CARTESIAN_POINT ( 'NONE',  ( -4.143013757418743559, 50.00090654753341823, -12.78394331335679013 ) ) ;
#20335 = CARTESIAN_POINT ( 'NONE',  ( 213.9946316566572193, 7.420549012114688203, -3.662783021451589960 ) ) ;
#20336 = VECTOR ( 'NONE', #16310, 1000.000000000000114 ) ;
#20337 = ORIENTED_EDGE ( 'NONE', *, *, #7090, .T. ) ;
#20338 = VERTEX_POINT ( 'NONE', #3632 ) ;
#20339 = FACE_OUTER_BOUND ( 'NONE', #1981, .T. ) ;
#20340 = DIRECTION ( 'NONE',  ( -0.000000000000000000, -1.000000000000000000, -0.000000000000000000 ) ) ;
#20341 = TOROIDAL_SURFACE ( 'NONE', #2760, 4.730184897849351700, 1.000000000000000000 ) ;
#20342 = CARTESIAN_POINT ( 'NONE',  ( 199.8561199650368110, 21.41935459518070317, -26.45271578590685380 ) ) ;
#20343 = EDGE_CURVE ( 'NONE', #2398, #3348, #15012, .T. ) ;
#20344 = VECTOR ( 'NONE', #12752, 1000.000000000000114 ) ;
#20345 = VECTOR ( 'NONE', #3776, 1000.000000000000000 ) ;
#20346 = LINE ( 'NONE', #17173, #5031 ) ;
#20347 = AXIS2_PLACEMENT_3D ( 'NONE', #19346, #16177, #6817 ) ;
#20348 = DIRECTION ( 'NONE',  ( -0.8660254037844362651, -0.5000000000000038858, 0.000000000000000000 ) ) ;
#20349 = PLANE ( 'NONE',  #879 ) ;
#20350 = DIRECTION ( 'NONE',  ( 0.000000000000000000, 0.000000000000000000, -1.000000000000000000 ) ) ;
#20351 = CARTESIAN_POINT ( 'NONE',  ( 200.4130575059754733, 6.471181724797008705, -24.79563718815128226 ) ) ;
#20352 = CARTESIAN_POINT ( 'NONE',  ( 202.6438527999323185, 0.8671737836725290638, -4.409371045252821197 ) ) ;
#20353 = DIRECTION ( 'NONE',  ( 0.4999999999999997224, -0.8660254037844388186, 0.000000000000000000 ) ) ;
#20354 = ORIENTED_EDGE ( 'NONE', *, *, #4953, .F. ) ;
#20355 = CARTESIAN_POINT ( 'NONE',  ( 81.30365475525482566, 58.89271721487809685, -1.003292558584042649 ) ) ;
#20356 = EDGE_CURVE ( 'NONE', #9189, #4251, #2056, .T. ) ;
#20357 = CIRCLE ( 'NONE', #9515, 1.000000000000000888 ) ;
#20358 = ORIENTED_EDGE ( 'NONE', *, *, #19194, .F. ) ;
#20359 = VERTEX_POINT ( 'NONE', #9878 ) ;
#20360 = DIRECTION ( 'NONE',  ( 0.5000000000000044409, -0.8660254037844360431, 0.000000000000000000 ) ) ;
#20361 = DIRECTION ( 'NONE',  ( 0.5000000000000054401, -0.8660254037844354880, 2.220446049250312834E-16 ) ) ;
#20362 = VECTOR ( 'NONE', #16202, 999.9999999999998863 ) ;
#20363 = VECTOR ( 'NONE', #10196, 1000.000000000000114 ) ;
#20364 = CARTESIAN_POINT ( 'NONE',  ( 0.000000000000000000, 0.000000000000000000, 0.000000000000000000 ) ) ;
#20365 = ADVANCED_FACE ( 'NONE', ( #5213 ), #18064, .F. ) ;
#20366 = DIRECTION ( 'NONE',  ( 1.000000000000000000, 0.000000000000000000, -1.153604387573318063E-16 ) ) ;
#20367 = ORIENTED_EDGE ( 'NONE', *, *, #652, .T. ) ;
#20368 = CARTESIAN_POINT ( 'NONE',  ( -46.99999999999998579, 65.00000000000000000, -12.50000000000000000 ) ) ;
#20369 = EDGE_CURVE ( 'NONE', #6269, #9819, #3531, .T. ) ;
#20370 = DIRECTION ( 'NONE',  ( 0.5000000000000057732, -0.8660254037844353769, 0.000000000000000000 ) ) ;
#20371 = DIRECTION ( 'NONE',  ( 0.000000000000000000, 0.000000000000000000, -1.000000000000000000 ) ) ;
#20372 = FACE_OUTER_BOUND ( 'NONE', #4767, .T. ) ;
#20373 =( GEOMETRIC_REPRESENTATION_CONTEXT ( 3 ) GLOBAL_UNCERTAINTY_ASSIGNED_CONTEXT ( ( #11475 ) ) GLOBAL_UNIT_ASSIGNED_CONTEXT ( ( #1003, #2809, #5858 ) ) REPRESENTATION_CONTEXT ( 'NONE', 'WORKASPACE' ) );
#20374 = DIRECTION ( 'NONE',  ( 0.5000000000000049960, -0.8660254037844358210, 0.000000000000000000 ) ) ;
#20375 = VECTOR ( 'NONE', #15852, 1000.000000000000114 ) ;
#20376 = CARTESIAN_POINT ( 'NONE',  ( 216.1221914169060199, 15.89489377461772079, -15.41371838795031657 ) ) ;
#20377 = DIRECTION ( 'NONE',  ( 0.8660254037844372643, 0.5000000000000025535, 0.000000000000000000 ) ) ;
#20378 = CARTESIAN_POINT ( 'NONE',  ( 199.2144802262915846, 21.04890371929339921, -14.00000000000005507 ) ) ;
#20379 = ORIENTED_EDGE ( 'NONE', *, *, #10019, .T. ) ;
#20380 = SURFACE_STYLE_FILL_AREA ( #3849 ) ;
#20381 = CARTESIAN_POINT ( 'NONE',  ( 4.000000000000000000, -1.759474945355387954, -3.047499999999997211 ) ) ;
#20382 = DIRECTION ( 'NONE',  ( 0.5000000000000052180, -0.8660254037844355990, -1.665334536937734071E-16 ) ) ;
#20383 = CARTESIAN_POINT ( 'NONE',  ( -14.95830009086074597, 79.99999999999985789, -12.45923801546573095 ) ) ;
#20385 = ORIENTED_EDGE ( 'NONE', *, *, #13634, .F. ) ;
#20384 = ORIENTED_EDGE ( 'NONE', *, *, #17329, .F. ) ;
#20386 = ORIENTED_EDGE ( 'NONE', *, *, #4208, .T. ) ;
#20387 = DIRECTION ( 'NONE',  ( -0.5000000000000049960, 0.8660254037844358210, -0.000000000000000000 ) ) ;
#20388 = CARTESIAN_POINT ( 'NONE',  ( 27.00000000000002487, 65.00000000000000000, -12.50000000000000000 ) ) ;
#20389 = ORIENTED_EDGE ( 'NONE', *, *, #3079, .F. ) ;
#20390 = FACE_OUTER_BOUND ( 'NONE', #2517, .T. ) ;
#20391 = PRODUCT_DEFINITION_CONTEXT ( 'detailed design', #17060, 'design' ) ;
#20392 = EDGE_CURVE ( 'NONE', #14976, #16924, #16371, .T. ) ;
#20393 = AXIS2_PLACEMENT_3D ( 'NONE', #8318, #11202, #11624 ) ;
#20394 = B_SPLINE_CURVE_WITH_KNOTS ( 'NONE', 3,
 ( #10828, #20376, #18793, #17311 ),
 .UNSPECIFIED., .F., .F.,
 ( 4, 4 ),
 ( 0.0001343368750301437032, 0.0008069876670732752024 ),
 .UNSPECIFIED. ) ;
#20395 = CARTESIAN_POINT ( 'NONE',  ( -34.66662763442661799, 64.25000000000000000, -1.859747928060479172 ) ) ;
#20396 = CARTESIAN_POINT ( 'NONE',  ( -28.99999999999999289, -10.00000000000000000, -15.00000000000000000 ) ) ;
#20397 = DIRECTION ( 'NONE',  ( 0.5000000000000051070, -0.8660254037844359321, 0.000000000000000000 ) ) ;
#20398 =( LENGTH_UNIT ( ) NAMED_UNIT ( * ) SI_UNIT ( .MILLI., .METRE. ) );
#20399 = EDGE_CURVE ( 'NONE', #16498, #16111, #1848, .T. ) ;
#20400 = ORIENTED_EDGE ( 'NONE', *, *, #19765, .T. ) ;
#20401 = CARTESIAN_POINT ( 'NONE',  ( 208.7495889232815216, 11.81532964447892375, -15.82564276083900445 ) ) ;
#20402 = CARTESIAN_POINT ( 'NONE',  ( -14.99999999999999645, -10.00000000000000000, 30.00000000000000000 ) ) ;
#20403 = CIRCLE ( 'NONE', #11279, 3.902363844300875240 ) ;
#20404 = LINE ( 'NONE', #7781, #10495 ) ;
#20405 = DIRECTION ( 'NONE',  ( 0.4999999999999995004, -0.8660254037844390407, 0.000000000000000000 ) ) ;
#20407 = ORIENTED_EDGE ( 'NONE', *, *, #15528, .T. ) ;
#20406 = EDGE_LOOP ( 'NONE', ( #18597, #10521, #8521, #9380 ) ) ;
#20408 = EDGE_LOOP ( 'NONE', ( #10074, #16358, #19641, #20718 ) ) ;
#20409 = LINE ( 'NONE', #5878, #19017 ) ;
#20410 = EDGE_CURVE ( 'NONE', #139, #8555, #6913, .T. ) ;
#20411 = VERTEX_POINT ( 'NONE', #6591 ) ;
#20412 = DIRECTION ( 'NONE',  ( 0.8660254037844370423, 0.5000000000000026645, -0.000000000000000000 ) ) ;
#20413 = PRODUCT_DEFINITION_SHAPE ( 'NONE', 'NONE',  #20958 ) ;
#20414 = CARTESIAN_POINT ( 'NONE',  ( 79.41606274153808442, 49.65173344286001367, -10.61500173657835155 ) ) ;
#20415 = LINE ( 'NONE', #10987, #19178 ) ;
#20416 = EDGE_CURVE ( 'NONE', #1588, #2098, #8291, .T. ) ;
#20417 = CARTESIAN_POINT ( 'NONE',  ( 190.1694833127194499, 64.25747545832879837, -14.00000000000006395 ) ) ;
#20418 = DIRECTION ( 'NONE',  ( -0.4711304610594118647, 0.8160218955482464454, -0.3348796121709901596 ) ) ;
#20419 = TOROIDAL_SURFACE ( 'NONE', #20765, 5.400000000000001243, 0.4000000000000000222 ) ;
#20420 = ORIENTED_EDGE ( 'NONE', *, *, #18992, .F. ) ;
#20421 = ORIENTED_EDGE ( 'NONE', *, *, #13976, .F. ) ;
#20422 = CARTESIAN_POINT ( 'NONE',  ( -15.99999999999999289, 80.00000000000000000, 12.50000000000000000 ) ) ;
#20423 = ADVANCED_FACE ( 'NONE', ( #17864 ), #7022, .T. ) ;
#20424 = EDGE_CURVE ( 'NONE', #18395, #2861, #13398, .T. ) ;
#20425 = DIRECTION ( 'NONE',  ( -0.8660254037844361541, -0.5000000000000045519, 5.976026924694054558E-17 ) ) ;
#20426 = CARTESIAN_POINT ( 'NONE',  ( -25.48018294944744611, 50.26343215275641541, -8.155225720970078029 ) ) ;
#20427 = DIRECTION ( 'NONE',  ( 0.000000000000000000, 6.938893903907177533E-18, 1.000000000000000000 ) ) ;
#20428 = CARTESIAN_POINT ( 'NONE',  ( 197.8194874830827814, 5.504832635710179112, -22.07143452975716258 ) ) ;
#20429 = CARTESIAN_POINT ( 'NONE',  ( 208.8748369350943506, 26.62631326558856060, -8.415281845792092597 ) ) ;
#20431 = ORIENTED_EDGE ( 'NONE', *, *, #12033, .T. ) ;
#20430 = ORIENTED_EDGE ( 'NONE', *, *, #15371, .F. ) ;
#20432 = AXIS2_PLACEMENT_3D ( 'NONE', #1701, #20778, #16 ) ;
#20433 = CARTESIAN_POINT ( 'NONE',  ( 221.4641624591582172, 32.64172757717244622, -12.10162843130820853 ) ) ;
#20434 = VECTOR ( 'NONE', #20559, 1000.000000000000000 ) ;
#20435 = CYLINDRICAL_SURFACE ( 'NONE', #3736, 12.47473710546057646 ) ;
#20436 = EDGE_CURVE ( 'NONE', #10831, #784, #10192, .T. ) ;
#20437 = EDGE_LOOP ( 'NONE', ( #6741, #17575, #14204, #6673, #16097 ) ) ;
#20438 = ORIENTED_EDGE ( 'NONE', *, *, #9644, .T. ) ;
#20439 = DIRECTION ( 'NONE',  ( 0.8660254037844375974, 0.5000000000000018874, 0.000000000000000000 ) ) ;
#20440 = DIRECTION ( 'NONE',  ( 0.000000000000000000, 0.000000000000000000, -1.000000000000000000 ) ) ;
#20441 = CARTESIAN_POINT ( 'NONE',  ( -0.3030695078776163842, 50.42519578546549042, -8.938776343028093763 ) ) ;
#20442 = CARTESIAN_POINT ( 'NONE',  ( -35.00000000000000000, 65.74999999999997158, -1.525597966176003961 ) ) ;
#20443 = EDGE_LOOP ( 'NONE', ( #18748, #12808 ) ) ;
#20444 = VERTEX_POINT ( 'NONE', #17960 ) ;
#20445 = CARTESIAN_POINT ( 'NONE',  ( 1.442378013833077732, 75.57646748667872316, -1.814718499151617870 ) ) ;
#20446 = ORIENTED_EDGE ( 'NONE', *, *, #629, .T. ) ;
#20447 = EDGE_CURVE ( 'NONE', #20827, #17781, #251, .T. ) ;
#20448 = CARTESIAN_POINT ( 'NONE',  ( 44.99529059433372424, 246.0222400402097946, -18.99999999999997513 ) ) ;
#20449 = CARTESIAN_POINT ( 'NONE',  ( 218.5362608324210782, 10.04265983930142347, -9.928836400542515150 ) ) ;
#20450 = CARTESIAN_POINT ( 'NONE',  ( -11.25987086420109229, 16.72409293340036385, 11.56718819196806791 ) ) ;
#20451 = CARTESIAN_POINT ( 'NONE',  ( 212.2886526734226607, 13.32755979150977943, -4.003039906354141308 ) ) ;
#20452 = CARTESIAN_POINT ( 'NONE',  ( 194.8843532073694291, 18.54890371929339565, -14.00000000000005507 ) ) ;
#20453 = CARTESIAN_POINT ( 'NONE',  ( 220.6963894288021493, 32.45804308600664001, -11.78314368930809763 ) ) ;
#20454 = DIRECTION ( 'NONE',  ( 0.000000000000000000, -0.5000000000000022204, -0.8660254037844372643 ) ) ;
#20455 = B_SPLINE_CURVE_WITH_KNOTS ( 'NONE', 3,
 ( #8515, #11488, #6915, #15015 ),
 .UNSPECIFIED., .F., .F.,
 ( 4, 4 ),
 ( 3.849233602880743113E-07, 0.0005858732790999119028 ),
 .UNSPECIFIED. ) ;
#20456 = CARTESIAN_POINT ( 'NONE',  ( -32.20403829709411525, 69.52210068921769448, 1.838693167884530633 ) ) ;
#20457 = FACE_OUTER_BOUND ( 'NONE', #4340, .T. ) ;
#20458 = CARTESIAN_POINT ( 'NONE',  ( -13.51899739228861463, 10.09941697557069595, 4.999999999999990230 ) ) ;
#20459 = EDGE_LOOP ( 'NONE', ( #10959, #16559, #3124, #17022, #10864, #13317, #16003, #1643, #20715, #6712, #9739 ) ) ;
#20460 = CARTESIAN_POINT ( 'NONE',  ( 80.11990493742565889, 66.91023862110843368, 0.3737492815355051845 ) ) ;
#20461 = ORIENTED_EDGE ( 'NONE', *, *, #4571, .F. ) ;
#20462 = EDGE_LOOP ( 'NONE', ( #20612, #15459, #3547, #11544 ) ) ;
#20463 = CARTESIAN_POINT ( 'NONE',  ( 0.8280627163074613106, 72.52289824211320024, 0.4796438872529771302 ) ) ;
#20464 = AXIS2_PLACEMENT_3D ( 'NONE', #7770, #17333, #14166 ) ;
#20465 = CARTESIAN_POINT ( 'NONE',  ( 227.5312376355471145, 39.64027283883993391, -14.00000000000005507 ) ) ;
#20466 = DIRECTION ( 'NONE',  ( 0.8660254037844353769, 0.5000000000000054401, -3.055037149610300800E-16 ) ) ;
#20467 = ORIENTED_EDGE ( 'NONE', *, *, #6403, .T. ) ;
#20468 = CARTESIAN_POINT ( 'NONE',  ( 207.4176018615384010, 11.04630655582441356, -12.09449022909012328 ) ) ;
#20469 = LINE ( 'NONE', #10821, #13503 ) ;
#20470 = CARTESIAN_POINT ( 'NONE',  ( 25.17200000000003612, 6.123233995736767268E-16, -5.000000000000000888 ) ) ;
#20471 = CARTESIAN_POINT ( 'NONE',  ( 34.99529059433364608, 263.3427481158985302, -28.99999999999997513 ) ) ;
#20472 = PLANE ( 'NONE',  #3133 ) ;
#20473 = SHAPE_REPRESENTATION ( 'Drill Bit Assembly Sliding Track Base', ( #18233 ), #20925 ) ;
#20474 = DIRECTION ( 'NONE',  ( 0.000000000000000000, 0.4999999999999983347, -0.8660254037844395958 ) ) ;
#20475 = LINE ( 'NONE', #1101, #10872 ) ;
#20476 = AXIS2_PLACEMENT_3D ( 'NONE', #12263, #13962, #15454 ) ;
#20477 = PLANE ( 'NONE',  #5331 ) ;
#20478 = VERTEX_POINT ( 'NONE', #13298 ) ;
#20479 = CARTESIAN_POINT ( 'NONE',  ( 209.4907977912994568, 12.24326678395481949, -15.16670265247205585 ) ) ;
#20480 = EDGE_CURVE ( 'NONE', #18381, #9665, #15429, .T. ) ;
#20481 = LINE ( 'NONE', #2800, #7797 ) ;
#20482 = EDGE_CURVE ( 'NONE', #10247, #17375, #10294, .T. ) ;
#20483 = CARTESIAN_POINT ( 'NONE',  ( 220.0968443491207722, 35.00999201386641602, -10.43865930680574827 ) ) ;
#20484 = CARTESIAN_POINT ( 'NONE',  ( 0.000000000000000000, -3.518949890710766581, 4.553649124439118623E-15 ) ) ;
#20486 = ORIENTED_EDGE ( 'NONE', *, *, #13273, .T. ) ;
#20485 = ORIENTED_EDGE ( 'NONE', *, *, #1844, .T. ) ;
#20487 = DIRECTION ( 'NONE',  ( 0.000000000000000000, -1.224646799147353454E-16, 1.000000000000000000 ) ) ;
#20488 = ORIENTED_EDGE ( 'NONE', *, *, #19362, .T. ) ;
#20489 = FACE_OUTER_BOUND ( 'NONE', #11487, .T. ) ;
#20490 = AXIS2_PLACEMENT_3D ( 'NONE', #20262, #13918, #4676 ) ;
#20491 = ORIENTED_EDGE ( 'NONE', *, *, #15264, .F. ) ;
#20492 = CARTESIAN_POINT ( 'NONE',  ( 195.8395605881523522, 4.361721309946301695, -9.913166705713630122 ) ) ;
#20493 = EDGE_CURVE ( 'NONE', #13116, #4077, #9051, .T. ) ;
#20494 = DIRECTION ( 'NONE',  ( -0.000000000000000000, -0.000000000000000000, 1.000000000000000000 ) ) ;
#20495 = ORIENTED_EDGE ( 'NONE', *, *, #14425, .T. ) ;
#20496 = CARTESIAN_POINT ( 'NONE',  ( 210.4326046345175314, 5.879217990898649049, -26.11230899909619652 ) ) ;
#20497 = LINE ( 'NONE', #19212, #32 ) ;
#20498 = CARTESIAN_POINT ( 'NONE',  ( 45.00000000000000000, -10.00000000000000000, 15.00000000000000000 ) ) ;
#20499 = AXIS2_PLACEMENT_3D ( 'NONE', #19442, #9690, #20926 ) ;
#20500 = DIRECTION ( 'NONE',  ( -0.8660254037844357100, -0.5000000000000051070, 0.000000000000000000 ) ) ;
#20501 = EDGE_CURVE ( 'NONE', #2200, #14662, #13506, .T. ) ;
#20502 = DIRECTION ( 'NONE',  ( -0.000000000000000000, 1.000000000000000000, -0.000000000000000000 ) ) ;
#20503 = VECTOR ( 'NONE', #14861, 1000.000000000000114 ) ;
#20504 = EDGE_CURVE ( 'NONE', #19519, #12506, #13825, .T. ) ;
#20505 = VERTEX_POINT ( 'NONE', #7019 ) ;
#20506 = ORIENTED_EDGE ( 'NONE', *, *, #10126, .F. ) ;
#20507 = VECTOR ( 'NONE', #20631, 1000.000000000000227 ) ;
#20508 = PLANE ( 'NONE',  #4116 ) ;
#20509 = ORIENTED_EDGE ( 'NONE', *, *, #7784, .T. ) ;
#20510 = DIRECTION ( 'NONE',  ( 0.5000000000000049960, -0.8660254037844357100, 0.000000000000000000 ) ) ;
#20511 = DIRECTION ( 'NONE',  ( 0.5000000000000053291, -0.8660254037844355990, -3.330669073875468142E-16 ) ) ;
#20512 = DIRECTION ( 'NONE',  ( -0.6299240516454518435, -0.3636868207865263103, 0.6862416378687374863 ) ) ;
#20513 = B_SPLINE_CURVE_WITH_KNOTS ( 'NONE', 3,
 ( #7721, #20445, #4446, #16013, #7823, #4341, #20758, #2756, #1477, #4548, #19179, #6326, #14324, #17487 ),
 .UNSPECIFIED., .F., .F.,
 ( 4, 2, 2, 2, 2, 2, 4 ),
 ( 0.000000000000000000, 0.003003218663418320920, 0.004504827995127496341, 0.006006437326836673064, 0.009009655990255062072, 0.01051126532196427869, 0.01201287465367349358 ),
 .UNSPECIFIED. ) ;
#20514 = EDGE_CURVE ( 'NONE', #862, #9014, #16888, .T. ) ;
#20515 = LINE ( 'NONE', #2835, #6937 ) ;
#20516 = CARTESIAN_POINT ( 'NONE',  ( 86.00000000000000000, 65.00000000000000000, -22.49999999999999645 ) ) ;
#20517 = VECTOR ( 'NONE', #18712, 1000.000000000000227 ) ;
#20518 = EDGE_LOOP ( 'NONE', ( #1931, #19561, #17995, #11784, #792, #13494 ) ) ;
#20519 = AXIS2_PLACEMENT_3D ( 'NONE', #13028, #5567, #11846 ) ;
#20520 = DIRECTION ( 'NONE',  ( -0.8528685319524407227, -0.4924038765061097833, -0.1736481776669268062 ) ) ;
#20521 = EDGE_CURVE ( 'NONE', #14504, #9868, #12123, .T. ) ;
#20522 = B_SPLINE_CURVE_WITH_KNOTS ( 'NONE', 3,
 ( #5784, #1241, #14189, #6199 ),
 .UNSPECIFIED., .F., .F.,
 ( 4, 4 ),
 ( 3.066983677343236917E-07, 0.0006729574904181037653 ),
 .UNSPECIFIED. ) ;
#20523 = CARTESIAN_POINT ( 'NONE',  ( 219.0213840155757907, 37.28461425646556648, -10.92122735228184460 ) ) ;
#20524 = CARTESIAN_POINT ( 'NONE',  ( -25.16391558800473760, 50.10856639097445253, -14.31252464806517821 ) ) ;
#20525 = CARTESIAN_POINT ( 'NONE',  ( 228.6507613633879430, 38.35419767703787386, -10.68456754651928087 ) ) ;
#20526 = EDGE_CURVE ( 'NONE', #1462, #627, #8929, .T. ) ;
#20527 = LINE ( 'NONE', #12490, #18614 ) ;
#20528 = CARTESIAN_POINT ( 'NONE',  ( -27.76344977743868370, 46.10015299616479467, -4.242667606105982259 ) ) ;
#20530 = EDGE_LOOP ( 'NONE', ( #4237, #20561 ) ) ;
#20529 = ORIENTED_EDGE ( 'NONE', *, *, #18506, .F. ) ;
#20531 = ORIENTED_EDGE ( 'NONE', *, *, #11677, .F. ) ;
#20532 = CARTESIAN_POINT ( 'NONE',  ( 0.000000000000000000, -2.342598717236899830, 4.057500000000059615 ) ) ;
#20533 = CARTESIAN_POINT ( 'NONE',  ( 212.8949410924155927, 14.03163993103081886, -5.166194743381471888 ) ) ;
#20534 = CARTESIAN_POINT ( 'NONE',  ( -3.197230184752320348, 76.40330993047184904, -2.758159894511169608 ) ) ;
#20535 = ORIENTED_EDGE ( 'NONE', *, *, #16934, .T. ) ;
#20536 = ORIENTED_EDGE ( 'NONE', *, *, #5131, .T. ) ;
#20537 = AXIS2_PLACEMENT_3D ( 'NONE', #3694, #10148, #3496 ) ;
#20538 = DIRECTION ( 'NONE',  ( 0.000000000000000000, 0.000000000000000000, 1.000000000000000000 ) ) ;
#20539 = PLANE ( 'NONE',  #16620 ) ;
#20540 = CARTESIAN_POINT ( 'NONE',  ( -33.40894099675318074, 52.30484166333695129, -4.500993475257865306 ) ) ;
#20541 = DIRECTION ( 'NONE',  ( 0.8660254037844370423, 0.5000000000000026645, -0.000000000000000000 ) ) ;
#20542 = ORIENTED_EDGE ( 'NONE', *, *, #18704, .F. ) ;
#20543 = ADVANCED_FACE ( 'NONE', ( #10726 ), #18379, .T. ) ;
#20544 = ADVANCED_FACE ( 'NONE', ( #12120, #883 ), #18695, .F. ) ;
#20545 = EDGE_LOOP ( 'NONE', ( #4434, #4566, #15972, #19953 ) ) ;
#20546 = CARTESIAN_POINT ( 'NONE',  ( 159.9952905943347901, 46.83639716978954226, -6.000000000000052403 ) ) ;
#20547 = VERTEX_POINT ( 'NONE', #3845 ) ;
#20548 = CARTESIAN_POINT ( 'NONE',  ( -15.99999999999999289, -9.999999999999994671, 4.999999999999989342 ) ) ;
#20549 = CARTESIAN_POINT ( 'NONE',  ( 229.2908607893598401, 36.91902289282235472, -11.99328011306290698 ) ) ;
#20550 = CARTESIAN_POINT ( 'NONE',  ( 75.92249532564342474, 71.86678175105188870, -24.92804124451842540 ) ) ;
#20551 = EDGE_CURVE ( 'NONE', #4202, #3563, #2006, .T. ) ;
#20552 = AXIS2_PLACEMENT_3D ( 'NONE', #17382, #12507, #19077 ) ;
#20553 = CARTESIAN_POINT ( 'NONE',  ( 22.00490953756710510, 255.8427481158984733, -28.99999999999997513 ) ) ;
#20554 = DIRECTION ( 'NONE',  ( 0.8660254037844369313, 0.5000000000000029976, -2.775557561562891351E-16 ) ) ;
#20555 = FACE_OUTER_BOUND ( 'NONE', #16128, .T. ) ;
#20556 = ORIENTED_EDGE ( 'NONE', *, *, #17326, .F. ) ;
#20557 = AXIS2_PLACEMENT_3D ( 'NONE', #2450, #15712, #14226 ) ;
#20558 = CARTESIAN_POINT ( 'NONE',  ( -28.70260728275128415, 67.76582539289573504, 2.255487788205997823 ) ) ;
#20559 = DIRECTION ( 'NONE',  ( 0.000000000000000000, 0.4999999999999983347, -0.8660254037844395958 ) ) ;
#20560 = DIRECTION ( 'NONE',  ( -0.3155439721630258765, 0.5465381918084566415, -0.7757112907044233507 ) ) ;
#20561 = ORIENTED_EDGE ( 'NONE', *, *, #13692, .T. ) ;
#20562 = ADVANCED_FACE ( 'NONE', ( #15218 ), #9030, .F. ) ;
#20563 = CARTESIAN_POINT ( 'NONE',  ( 75.06454086321275554, 72.57489325992457907, -0.2429554351602942197 ) ) ;
#20564 = ORIENTED_EDGE ( 'NONE', *, *, #16294, .F. ) ;
#20565 = EDGE_LOOP ( 'NONE', ( #999, #19890, #3364, #2173 ) ) ;
#20566 = DIRECTION ( 'NONE',  ( 0.8660254037844370423, 0.5000000000000026645, -0.000000000000000000 ) ) ;
#20567 = CARTESIAN_POINT ( 'NONE',  ( 5.000000000000000000, 0.000000000000000000, 0.000000000000000000 ) ) ;
#20568 = VECTOR ( 'NONE', #20418, 1000.000000000000114 ) ;
#20569 = APPLICATION_PROTOCOL_DEFINITION ( 'draft international standard', 'automotive_design', 1998, #16246 ) ;
#20570 =( REPRESENTATION_RELATIONSHIP ('NONE','NONE', #4634, #1796 ) REPRESENTATION_RELATIONSHIP_WITH_TRANSFORMATION ( #19099 )SHAPE_REPRESENTATION_RELATIONSHIP( ) );
#20571 = CIRCLE ( 'NONE', #11438, 11.94520687646042667 ) ;
#20572 = DIRECTION ( 'NONE',  ( -0.5000000000000049960, 0.8660254037844358210, -0.000000000000000000 ) ) ;
#20573 = EDGE_LOOP ( 'NONE', ( #17396, #19302, #17352 ) ) ;
#20574 = PRESENTATION_STYLE_ASSIGNMENT (( #1191 ) ) ;
#20575 = ORIENTED_EDGE ( 'NONE', *, *, #10011, .T. ) ;
#20576 = CYLINDRICAL_SURFACE ( 'NONE', #297, 5.000000000000002665 ) ;
#20577 = CYLINDRICAL_SURFACE ( 'NONE', #5930, 4.999999999999990230 ) ;
#20578 = DIRECTION ( 'NONE',  ( 0.5000000000000057732, -0.8660254037844352659, -1.942890293094023699E-16 ) ) ;
#20579 = DIRECTION ( 'NONE',  ( -0.8660254037844369313, -0.5000000000000027756, 0.000000000000000000 ) ) ;
#20580 = PLANE ( 'NONE',  #19086 ) ;
#20581 = CARTESIAN_POINT ( 'NONE',  ( 191.1694443951678295, 35.60712985292573052, -9.000000000000063949 ) ) ;
#20582 = VECTOR ( 'NONE', #15585, 1000.000000000000114 ) ;
#20583 = CARTESIAN_POINT ( 'NONE',  ( 204.6278860547989780, 24.17433503161487351, -24.79563718815146345 ) ) ;
#20584 = ORIENTED_EDGE ( 'NONE', *, *, #19135, .T. ) ;
#20585 = CARTESIAN_POINT ( 'NONE',  ( 229.6155621620580973, 37.00958275052409618, -11.94979443502199956 ) ) ;
#20587 = CARTESIAN_POINT ( 'NONE',  ( 199.3993387870319509, 20.72871929987707063, -14.00000000000005507 ) ) ;
#20586 =( GEOMETRIC_REPRESENTATION_CONTEXT ( 3 ) GLOBAL_UNCERTAINTY_ASSIGNED_CONTEXT ( ( #20595 ) ) GLOBAL_UNIT_ASSIGNED_CONTEXT ( ( #1009, #7454, #18814 ) ) REPRESENTATION_CONTEXT ( 'NONE', 'WORKASPACE' ) );
#20588 = DIRECTION ( 'NONE',  ( -0.5000000000000049960, 0.8660254037844357100, -0.000000000000000000 ) ) ;
#20589 = DIRECTION ( 'NONE',  ( -0.8660254037844361541, -0.5000000000000042188, 6.872020471724001723E-17 ) ) ;
#20591 = ORIENTED_EDGE ( 'NONE', *, *, #20882, .F. ) ;
#20590 = ORIENTED_EDGE ( 'NONE', *, *, #9117, .T. ) ;
#20592 = CARTESIAN_POINT ( 'NONE',  ( 221.8748702755764555, 32.34223107544470821, -12.52024606262113693 ) ) ;
#20593 = CARTESIAN_POINT ( 'NONE',  ( 213.8895336909654361, 8.132690763974602888, -24.79563718815146345 ) ) ;
#20594 = ORIENTED_EDGE ( 'NONE', *, *, #8634, .F. ) ;
#20595 = UNCERTAINTY_MEASURE_WITH_UNIT (LENGTH_MEASURE( 1.000000000000000082E-05 ), #1009, 'distance_accuracy_value', 'NONE');
#20596 = CARTESIAN_POINT ( 'NONE',  ( 70.73635393167552365, 76.06156464907579107, -23.63261108224246243 ) ) ;
#20597 = VECTOR ( 'NONE', #1313, 1000.000000000000114 ) ;
#20598 = ORIENTED_EDGE ( 'NONE', *, *, #18582, .F. ) ;
#20599 = DIRECTION ( 'NONE',  ( 0.8660254037844370423, 0.5000000000000026645, -0.000000000000000000 ) ) ;
#20600 = LINE ( 'NONE', #12460, #14743 ) ;
#20601 = ORIENTED_EDGE ( 'NONE', *, *, #20680, .T. ) ;
#20602 = SHAPE_REPRESENTATION ( 'socket head cap screw_iso_ISO 4762 M10 x 70 - 32N', ( #18233 ), #20586 ) ;
#20603 = ADVANCED_FACE ( 'NONE', ( #2367 ), #10619, .T. ) ;
#20604 = FACE_OUTER_BOUND ( 'NONE', #18246, .T. ) ;
#20605 =( NAMED_UNIT ( * ) PLANE_ANGLE_UNIT ( ) SI_UNIT ( $, .RADIAN. ) );
#20606 = ORIENTED_EDGE ( 'NONE', *, *, #2292, .F. ) ;
#20607 = DIRECTION ( 'NONE',  ( 0.5000000000000034417, -0.8660254037844364872, 0.000000000000000000 ) ) ;
#20608 = DIRECTION ( 'NONE',  ( -0.7235536692358655042, -0.4177439057064740169, -0.5495089780708011240 ) ) ;
#20609 = DIRECTION ( 'NONE',  ( 0.000000000000000000, 0.000000000000000000, 1.000000000000000000 ) ) ;
#20610 = CARTESIAN_POINT ( 'NONE',  ( 0.3999999999999975797, 0.000000000000000000, 0.000000000000000000 ) ) ;
#20611 = AXIS2_PLACEMENT_3D ( 'NONE', #20947, #12932, #11332 ) ;
#20612 = ORIENTED_EDGE ( 'NONE', *, *, #5564, .F. ) ;
#20613 = FACE_OUTER_BOUND ( 'NONE', #4019, .T. ) ;
#20614 = EDGE_CURVE ( 'NONE', #19267, #8753, #16998, .T. ) ;
#20615 = ORIENTED_EDGE ( 'NONE', *, *, #7916, .T. ) ;
#20616 = DIRECTION ( 'NONE',  ( 0.5000000000000052180, -0.8660254037844355990, -0.000000000000000000 ) ) ;
#20617 = CARTESIAN_POINT ( 'NONE',  ( 79.78494060632117169, 50.66488423061860402, -7.505244347833114560 ) ) ;
#20618 = DIRECTION ( 'NONE',  ( 0.7366891686653871396, 0.000000000000000000, 0.6762315200958181061 ) ) ;
#20619 = DIRECTION ( 'NONE',  ( 1.000000000000000000, 0.000000000000000000, 0.000000000000000000 ) ) ;
#20620 = CARTESIAN_POINT ( 'NONE',  ( 207.0125913935839606, 3.389466186736467268, -25.65046807331631129 ) ) ;
#20621 = EDGE_CURVE ( 'NONE', #5527, #17966, #11790, .T. ) ;
#20622 = ORIENTED_EDGE ( 'NONE', *, *, #20170, .T. ) ;
#20623 = VECTOR ( 'NONE', #7799, 1000.000000000000227 ) ;
#20624 = EDGE_CURVE ( 'NONE', #16239, #2143, #9304, .T. ) ;
#20625 = CARTESIAN_POINT ( 'NONE',  ( 197.5592321514251353, 4.823524888127141530, -22.03054070023847544 ) ) ;
#20626 = FACE_BOUND ( 'NONE', #9630, .T. ) ;
#20627 = CARTESIAN_POINT ( 'NONE',  ( -8.070106850684350519, 45.02467605610512891, -9.668770963353599868 ) ) ;
#20628 = DIRECTION ( 'NONE',  ( -0.8660254037844370423, -0.5000000000000026645, 0.000000000000000000 ) ) ;
#20629 = B_SPLINE_CURVE_WITH_KNOTS ( 'NONE', 3,
 ( #13667, #18537, #17054, #18640, #17254, #13987, #4117, #20119, #5581, #4006, #10777, #10455, #2427, #4425, #17153, #10668, #2739, #13874, #8881, #20324, #2638, #1153, #7600, #14092, #20528, #5998, #2946, #17470, #9598, #20940, #14513, #4839, #6517, #4533, #6209, #4938, #17777, #9386, #1254, #9494, #13015, #6103, #11412, #17683, #11002, #17574 ),
 .UNSPECIFIED., .F., .F.,
 ( 4, 2, 2, 2, 2, 2, 2, 2, 2, 2, 2, 2, 2, 2, 2, 2, 2, 2, 2, 2, 2, 2, 4 ),
 ( 0.000000000000000000, 0.002324142326026098875, 0.004648284652052197749, 0.006972426978078296624, 0.009296569304104395498, 0.01162071163013049524, 0.01394485395615659325, 0.01510692511916964312, 0.01626899628218269125, 0.01859313860820877365, 0.01975520977122182179, 0.02091728093423487339, 0.02207935209724792153, 0.02324142326026096966, 0.02556556558628706247, 0.02672763674930011060, 0.02788970791231315527, 0.02905177907532619647, 0.03021385023833924460, 0.03253799256436533394, 0.03370006372737838207, 0.03486213489039143021, 0.03718627721641753342 ),
 .UNSPECIFIED. ) ;
#20630 = DIRECTION ( 'NONE',  ( -0.5000000000000045519, 0.8660254037844360431, 0.000000000000000000 ) ) ;
#20631 = DIRECTION ( 'NONE',  ( -0.5000000000000049960, 0.8660254037844358210, -0.000000000000000000 ) ) ;
#20633 = ORIENTED_EDGE ( 'NONE', *, *, #2865, .F. ) ;
#20632 = ORIENTED_EDGE ( 'NONE', *, *, #16814, .F. ) ;
#20634 = DIRECTION ( 'NONE',  ( -0.8660254037844359321, -0.5000000000000045519, 5.976026924694053325E-17 ) ) ;
#20635 = FACE_OUTER_BOUND ( 'NONE', #11135, .T. ) ;
#20636 = CARTESIAN_POINT ( 'NONE',  ( -2.552085020148435301, 77.20859777394468892, -3.699063880715907526 ) ) ;
#20637 = ORIENTED_EDGE ( 'NONE', *, *, #7828, .F. ) ;
#20638 = VERTEX_POINT ( 'NONE', #11916 ) ;
#20639 = LINE ( 'NONE', #18757, #6808 ) ;
#20640 = CARTESIAN_POINT ( 'NONE',  ( 4.000000000000000000, 1.759474945355388398, 3.047499999999996767 ) ) ;
#20641 = CARTESIAN_POINT ( 'NONE',  ( -8.315537089352744715, 50.19654607572633154, -14.93280926764117922 ) ) ;
#20642 = TOROIDAL_SURFACE ( 'NONE', #9797, 4.730184897849351700, 1.000000000000000000 ) ;
#20643 = FACE_OUTER_BOUND ( 'NONE', #4870, .T. ) ;
#20644 = EDGE_LOOP ( 'NONE', ( #4552, #15765 ) ) ;
#20645 = EDGE_CURVE ( 'NONE', #20444, #13693, #4377, .T. ) ;
#20646 = VECTOR ( 'NONE', #20630, 1000.000000000000114 ) ;
#20647 = ORIENTED_EDGE ( 'NONE', *, *, #20773, .T. ) ;
#20648 = DIRECTION ( 'NONE',  ( 0.000000000000000000, -0.8660254037844393737, -0.4999999999999987232 ) ) ;
#20649 = ADVANCED_FACE ( 'NONE', ( #3105 ), #1200, .F. ) ;
#20650 = CARTESIAN_POINT ( 'NONE',  ( 200.1915427753721417, 0.2241520214996718663, -5.993340328401664863 ) ) ;
#20651 = CARTESIAN_POINT ( 'NONE',  ( 226.0207045282809872, 42.90958974223701716, -14.96398743228909645 ) ) ;
#20652 = CARTESIAN_POINT ( 'NONE',  ( 4.000000000000000000, 0.000000000000000000, 0.000000000000000000 ) ) ;
#20653 = EDGE_CURVE ( 'NONE', #19461, #527, #9392, .T. ) ;
#20654 = CARTESIAN_POINT ( 'NONE',  ( 229.5766059392757086, 36.42409777515187841, -13.96704429371395229 ) ) ;
#20655 = PLANE ( 'NONE',  #20557 ) ;
#20656 = DIRECTION ( 'NONE',  ( -0.000000000000000000, 1.000000000000000000, -0.000000000000000000 ) ) ;
#20657 = AXIS2_PLACEMENT_3D ( 'NONE', #3634, #10194, #13301 ) ;
#20658 = ORIENTED_EDGE ( 'NONE', *, *, #4172, .F. ) ;
#20659 = LINE ( 'NONE', #14432, #11451 ) ;
#20660 = VECTOR ( 'NONE', #15860, 1000.000000000000227 ) ;
#20661 = PLANE ( 'NONE',  #19747 ) ;
#20662 = CARTESIAN_POINT ( 'NONE',  ( 229.3446640726370731, 37.47879200507496478, -16.31968669809504036 ) ) ;
#20663 = ADVANCED_FACE ( 'NONE', ( #12654 ), #17313, .T. ) ;
#20664 = ORIENTED_EDGE ( 'NONE', *, *, #5201, .F. ) ;
#20665 = CARTESIAN_POINT ( 'NONE',  ( 76.76720986645948130, 67.98148330769186032, 0.1575026721056629053 ) ) ;
#20666 = VECTOR ( 'NONE', #4647, 1000.000000000000000 ) ;
#20667 = EDGE_LOOP ( 'NONE', ( #20226, #1209, #20155, #19607, #4915, #15493 ) ) ;
#20668 = EDGE_LOOP ( 'NONE', ( #12508, #119, #19076 ) ) ;
#20669 = CARTESIAN_POINT ( 'NONE',  ( -3.061148255020639919, 72.78546382685976823, 0.3359787457721644111 ) ) ;
#20670 = LINE ( 'NONE', #1293, #10343 ) ;
#20671 = ADVANCED_FACE ( 'NONE', ( #2896 ), #1413, .F. ) ;
#20672 = VECTOR ( 'NONE', #9647, 1000.000000000000000 ) ;
#20673 = ITEM_DEFINED_TRANSFORMATION ( 'NONE', 'NONE', #6694,  #18233 ) ;
#20674 = AXIS2_PLACEMENT_3D ( 'NONE', #11636, #18099, #17899 ) ;
#20675 = CIRCLE ( 'NONE', #15952, 9.999999999999994671 ) ;
#20676 = FACE_OUTER_BOUND ( 'NONE', #12559, .T. ) ;
#20677 = ORIENTED_EDGE ( 'NONE', *, *, #2807, .T. ) ;
#20678 = CARTESIAN_POINT ( 'NONE',  ( 44.00000000000000000, 0.000000000000000000, 15.00000000000000000 ) ) ;
#20679 = ADVANCED_FACE ( 'NONE', ( #12446 ), #10830, .F. ) ;
#20680 = EDGE_CURVE ( 'NONE', #5956, #3195, #3000, .T. ) ;
#20681 = CARTESIAN_POINT ( 'NONE',  ( 215.9737506317248119, 15.45515208972567756, -9.718744748713270099 ) ) ;
#20682 = CARTESIAN_POINT ( 'NONE',  ( 210.3241885033056917, 28.95566150434252961, -16.41972909894644417 ) ) ;
#20683 = CARTESIAN_POINT ( 'NONE',  ( 0.05361705196957869402, 61.53954601429751392, 2.100564191518395241 ) ) ;
#20684 = AXIS2_PLACEMENT_3D ( 'NONE', #15657, #15760, #14282 ) ;
#20685 = ORIENTED_EDGE ( 'NONE', *, *, #11253, .T. ) ;
#20686 = DIRECTION ( 'NONE',  ( -0.3886714912512299613, -0.2243995901002340809, -0.8936326403234116089 ) ) ;
#20687 = CARTESIAN_POINT ( 'NONE',  ( 202.0496559082686474, 12.07111943211142169, -2.341985411376943826 ) ) ;
#20688 = ADVANCED_FACE ( 'NONE', ( #2796 ), #2659, .F. ) ;
#20689 = AXIS2_PLACEMENT_3D ( 'NONE', #4920, #3138, #683 ) ;
#20690 = CARTESIAN_POINT ( 'NONE',  ( 218.3074569161917964, 38.52117226549894724, -12.94403591235888840 ) ) ;
#20691 = DIRECTION ( 'NONE',  ( -0.5566703992264087075, -0.3213938048432681271, 0.7660444431189863401 ) ) ;
#20692 = EDGE_CURVE ( 'NONE', #18575, #7909, #4588, .T. ) ;
#20693 = DIRECTION ( 'NONE',  ( -0.6634139481689351747, -0.3830222215594923374, 0.6427876096865405842 ) ) ;
#20694 = ORIENTED_EDGE ( 'NONE', *, *, #18315, .F. ) ;
#20695 = AXIS2_PLACEMENT_3D ( 'NONE', #13941, #7343, #18705 ) ;
#20696 = LINE ( 'NONE', #17419, #15278 ) ;
#20697 = CARTESIAN_POINT ( 'NONE',  ( 205.2286857969292839, 9.782535276688832937, -15.28568448904319510 ) ) ;
#20698 = AXIS2_PLACEMENT_3D ( 'NONE', #5017, #13098, #12888 ) ;
#20699 = PLANE ( 'NONE',  #3042 ) ;
#20700 = DIRECTION ( 'NONE',  ( 0.000000000000000000, 0.000000000000000000, -1.000000000000000000 ) ) ;
#20701 = DIRECTION ( 'NONE',  ( -0.8660254037844380415, -0.5000000000000014433, -0.000000000000000000 ) ) ;
#20702 = APPLICATION_CONTEXT ( 'automotive_design' ) ;
#20703 = ADVANCED_FACE ( 'NONE', ( #7864 ), #20477, .F. ) ;
#20705 = ORIENTED_EDGE ( 'NONE', *, *, #20243, .F. ) ;
#20704 = ORIENTED_EDGE ( 'NONE', *, *, #9505, .F. ) ;
#20706 = CARTESIAN_POINT ( 'NONE',  ( 205.0662616026534693, 10.91332106064940888, -14.00000000000005507 ) ) ;
#20707 = DIRECTION ( 'NONE',  ( -1.000000000000000000, -0.000000000000000000, -0.000000000000000000 ) ) ;
#20708 = DIRECTION ( 'NONE',  ( -1.000000000000000000, -0.000000000000000000, -0.000000000000000000 ) ) ;
#20709 = LINE ( 'NONE', #5966, #17541 ) ;
#20710 = VECTOR ( 'NONE', #10600, 1000.000000000000227 ) ;
#20711 = EDGE_CURVE ( 'NONE', #3563, #8008, #434, .T. ) ;
#20712 = VECTOR ( 'NONE', #15009, 1000.000000000000000 ) ;
#20713 = LINE ( 'NONE', #6182, #1515 ) ;
#20714 = ORIENTED_EDGE ( 'NONE', *, *, #17264, .F. ) ;
#20715 = ORIENTED_EDGE ( 'NONE', *, *, #20482, .T. ) ;
#20716 = CARTESIAN_POINT ( 'NONE',  ( 99.99529059433426426, 150.7594456239217777, 1.000000000000008438 ) ) ;
#20717 =( LENGTH_UNIT ( ) NAMED_UNIT ( * ) SI_UNIT ( .MILLI., .METRE. ) );
#20718 = ORIENTED_EDGE ( 'NONE', *, *, #1852, .T. ) ;
#20719 = CARTESIAN_POINT ( 'NONE',  ( 199.4574108924007305, -0.1996992187545574282, -7.132002368301175288 ) ) ;
#20720 = CARTESIAN_POINT ( 'NONE',  ( 208.4761278624580711, 5.007259451653140125, -14.00000000000005507 ) ) ;
#20721 = CARTESIAN_POINT ( 'NONE',  ( 227.5312376355471145, 39.64027283883993391, -14.00000000000005507 ) ) ;
#20722 = CARTESIAN_POINT ( 'NONE',  ( 5.000000000000004441, -4.685197434473809430, 6.071532165918824830E-15 ) ) ;
#20723 = ORIENTED_EDGE ( 'NONE', *, *, #2261, .F. ) ;
#20724 = DIRECTION ( 'NONE',  ( -0.8660254037844360431, -0.5000000000000045519, 5.976026924694054558E-17 ) ) ;
#20725 = CIRCLE ( 'NONE', #18692, 12.50000000000000000 ) ;
#20726 = CIRCLE ( 'NONE', #4484, 11.94520687646042667 ) ;
#20727 = ORIENTED_EDGE ( 'NONE', *, *, #1240, .F. ) ;
#20728 = EDGE_CURVE ( 'NONE', #1051, #15696, #13381, .T. ) ;
#20729 = CARTESIAN_POINT ( 'NONE',  ( 220.2899471553721753, 34.67552814235484959, -10.49174204642378605 ) ) ;
#20730 = DIRECTION ( 'NONE',  ( -0.8528685319524385022, -0.4924038765061083955, 0.1736481776669413224 ) ) ;
#20731 = DIRECTION ( 'NONE',  ( 0.8660254037844355990, 0.5000000000000054401, 0.000000000000000000 ) ) ;
#20732 = CARTESIAN_POINT ( 'NONE',  ( -14.99999999999999645, -9.999999999999998224, 15.00000000000000000 ) ) ;
#20733 = DIRECTION ( 'NONE',  ( 0.4895420438411642317, -0.8479116923740014355, -0.2034560130526309740 ) ) ;
#20734 = ORIENTED_EDGE ( 'NONE', *, *, #7174, .T. ) ;
#20735 = CARTESIAN_POINT ( 'NONE',  ( 201.5316478576734198, 7.294022845898723517, -25.30691987834790524 ) ) ;
#20736 = AXIS2_PLACEMENT_3D ( 'NONE', #13793, #4350, #10918 ) ;
#20737 = AXIS2_PLACEMENT_3D ( 'NONE', #12161, #15257, #5250 ) ;
#20738 = CARTESIAN_POINT ( 'NONE',  ( -2.492300918882593308, 50.02397455645809998, -11.50064407951557222 ) ) ;
#20739 = DIRECTION ( 'NONE',  ( 0.5000000000000045519, -0.8660254037844361541, 0.000000000000000000 ) ) ;
#20740 = CARTESIAN_POINT ( 'NONE',  ( 106.8149328581056352, 188.4071680446163555, 11.00000000000001066 ) ) ;
#20741 = CARTESIAN_POINT ( 'NONE',  ( 98.22787951438910170, 199.6642187277107041, 13.37143655376591767 ) ) ;
#20743 = ORIENTED_EDGE ( 'NONE', *, *, #4956, .T. ) ;
#20742 = ORIENTED_EDGE ( 'NONE', *, *, #13487, .T. ) ;
#20744 = DIRECTION ( 'NONE',  ( 0.000000000000000000, -1.000000000000000000, 1.232415585510385534E-15 ) ) ;
#20745 = DIRECTION ( 'NONE',  ( -0.8660254037844360431, -0.5000000000000044409, 5.976026924694052093E-17 ) ) ;
#20746 = CARTESIAN_POINT ( 'NONE',  ( -3.032950703231028555, 76.49637892407336892, -2.857129582000850210 ) ) ;
#20747 = ORIENTED_EDGE ( 'NONE', *, *, #14356, .F. ) ;
#20748 = ORIENTED_EDGE ( 'NONE', *, *, #18479, .T. ) ;
#20749 = ORIENTED_EDGE ( 'NONE', *, *, #4022, .T. ) ;
#20750 = EDGE_CURVE ( 'NONE', #8276, #5621, #7545, .T. ) ;
#20751 = DIRECTION ( 'NONE',  ( -0.8660254037844359321, -0.5000000000000045519, 5.976026924694053325E-17 ) ) ;
#20752 = LINE ( 'NONE', #9398, #15955 ) ;
#20753 = CARTESIAN_POINT ( 'NONE',  ( -6.164506467296446246, 50.07147070244224096, -13.99886338058812640 ) ) ;
#20754 = DIRECTION ( 'NONE',  ( 0.8660254037844372643, 0.5000000000000027756, -0.000000000000000000 ) ) ;
#20755 = VECTOR ( 'NONE', #418, 1000.000000000000114 ) ;
#20756 = ORIENTED_EDGE ( 'NONE', *, *, #19895, .T. ) ;
#20757 = ORIENTED_EDGE ( 'NONE', *, *, #1196, .F. ) ;
#20758 = CARTESIAN_POINT ( 'NONE',  ( 0.7048535361513451614, 71.96725945621673759, 0.7929198755315660652 ) ) ;
#20759 = CARTESIAN_POINT ( 'NONE',  ( 221.5594486299148400, 33.09453545750766779, -16.83383072344321718 ) ) ;
#20760 = EDGE_CURVE ( 'NONE', #7899, #1475, #12191, .T. ) ;
#20761 = CARTESIAN_POINT ( 'NONE',  ( 229.4823745501375072, 36.26080457024635706, -13.97349461567483608 ) ) ;
#20762 = DIRECTION ( 'NONE',  ( 0.5000000000000007772, -0.8660254037844381525, 0.000000000000000000 ) ) ;
#20763 = CARTESIAN_POINT ( 'NONE',  ( 75.60538121466899497, 68.57595208612733018, -25.00629774707486419 ) ) ;
#20764 = AXIS2_PLACEMENT_3D ( 'NONE', #15706, #15596, #15498 ) ;
#20765 = AXIS2_PLACEMENT_3D ( 'NONE', #11267, #19507, #6566 ) ;
#20766 = ORIENTED_EDGE ( 'NONE', *, *, #19628, .T. ) ;
#20767 = CARTESIAN_POINT ( 'NONE',  ( 80.00000000000000000, 0.000000000000000000, 0.000000000000000000 ) ) ;
#20768 = DIRECTION ( 'NONE',  ( 0.000000000000000000, -0.000000000000000000, -1.000000000000000000 ) ) ;
#20769 = ORIENTED_EDGE ( 'NONE', *, *, #13036, .T. ) ;
#20770 = CARTESIAN_POINT ( 'NONE',  ( 82.31649210851065845, 65.12786813035249622, 0.6330763717910036226 ) ) ;
#20771 = EDGE_CURVE ( 'NONE', #11761, #3050, #18893, .T. ) ;
#20772 = ORIENTED_EDGE ( 'NONE', *, *, #15875, .T. ) ;
#20773 = EDGE_CURVE ( 'NONE', #19461, #17095, #18767, .T. ) ;
#20774 = ORIENTED_EDGE ( 'NONE', *, *, #3043, .T. ) ;
#20775 = CARTESIAN_POINT ( 'NONE',  ( -3.273749048447422538, 68.32062926339912678, 2.141136792363729668 ) ) ;
#20776 = LINE ( 'NONE', #17295, #4600 ) ;
#20777 = SHAPE_DEFINITION_REPRESENTATION ( #2657, #9638 ) ;
#20778 = DIRECTION ( 'NONE',  ( -0.5000000000000051070, 0.8660254037844359321, -0.000000000000000000 ) ) ;
#20779 = EDGE_CURVE ( 'NONE', #15885, #11656, #19551, .T. ) ;
#20780 = EDGE_LOOP ( 'NONE', ( #12860, #12810 ) ) ;
#20781 = CARTESIAN_POINT ( 'NONE',  ( -14.99999999999999645, 5.000000000000000000, -30.00000000000000000 ) ) ;
#20782 = DIRECTION ( 'NONE',  ( -0.5000000000000039968, 0.8660254037844363761, 0.000000000000000000 ) ) ;
#20783 = LINE ( 'NONE', #1404, #196 ) ;
#20784 = PLANE ( 'NONE',  #17310 ) ;
#20785 = CARTESIAN_POINT ( 'NONE',  ( 182.3972143829817867, 2.035126980567763866, -22.00000000000009948 ) ) ;
#20786 = DIRECTION ( 'NONE',  ( -0.8660254037844360431, -0.5000000000000044409, -4.336808689942049290E-16 ) ) ;
#20787 = EDGE_CURVE ( 'NONE', #19103, #17088, #750, .T. ) ;
#20788 = CARTESIAN_POINT ( 'NONE',  ( 193.8244552494320772, 17.93697134796469328, -3.188775577416750995 ) ) ;
#20789 = DIRECTION ( 'NONE',  ( 0.7951984747223578287, 0.4591080534401396629, -0.3960797660391672803 ) ) ;
#20790 = CARTESIAN_POINT ( 'NONE',  ( 202.7150726112346319, 7.800250765496993033, -25.94618751764486575 ) ) ;
#20791 = ORIENTED_EDGE ( 'NONE', *, *, #992, .F. ) ;
#20792 = VECTOR ( 'NONE', #7981, 1000.000000000000227 ) ;
#20793 = DIRECTION ( 'NONE',  ( 0.5000000000000045519, -0.8660254037844360431, 0.000000000000000000 ) ) ;
#20794 = EDGE_CURVE ( 'NONE', #9080, #688, #4020, .T. ) ;
#20795 = CARTESIAN_POINT ( 'NONE',  ( 70.67931723492910123, 76.10686176109747691, -1.383828600441279866 ) ) ;
#20796 = DIRECTION ( 'NONE',  ( 0.000000000000000000, -1.000000000000000000, 0.000000000000000000 ) ) ;
#20797 = CARTESIAN_POINT ( 'NONE',  ( -20.90971454361231352, 15.43716950431552171, 0.9458874751258853353 ) ) ;
#20799 = ORIENTED_EDGE ( 'NONE', *, *, #14721, .T. ) ;
#20798 = ORIENTED_EDGE ( 'NONE', *, *, #7718, .T. ) ;
#20800 = CARTESIAN_POINT ( 'NONE',  ( 209.4254563108873413, 4.782534396259779719, -0.8632678296711639998 ) ) ;
#20801 = UNCERTAINTY_MEASURE_WITH_UNIT (LENGTH_MEASURE( 1.000000000000000082E-05 ), #20084, 'distance_accuracy_value', 'NONE');
#20802 = EDGE_CURVE ( 'NONE', #7653, #385, #10315, .T. ) ;
#20803 = CARTESIAN_POINT ( 'NONE',  ( 219.6446699912483780, 35.99909917638625245, -17.59730712095013772 ) ) ;
#20804 = EDGE_CURVE ( 'NONE', #15949, #1882, #5700, .T. ) ;
#20805 = ORIENTED_EDGE ( 'NONE', *, *, #3899, .F. ) ;
#20806 = CARTESIAN_POINT ( 'NONE',  ( -32.03950703498303909, 78.52235084885765559, -5.999488569659933823 ) ) ;
#20807 = CARTESIAN_POINT ( 'NONE',  ( 61.99529059433388767, 216.5773763115390693, 1.000000000000017097 ) ) ;
#20808 = FACE_OUTER_BOUND ( 'NONE', #18895, .T. ) ;
#20809 = EDGE_CURVE ( 'NONE', #14614, #2046, #10050, .T. ) ;
#20810 = ORIENTED_EDGE ( 'NONE', *, *, #3142, .T. ) ;
#20811 = DIRECTION ( 'NONE',  ( -0.8660254037843260200, -0.5000000000001951772, 0.000000000000000000 ) ) ;
#20812 = CARTESIAN_POINT ( 'NONE',  ( 219.0593366061551137, 10.34465777807333531, -13.97827067520052147 ) ) ;
#20813 = APPLICATION_CONTEXT ( 'automotive_design' ) ;
#20814 = CARTESIAN_POINT ( 'NONE',  ( 227.5678821218066901, 40.55626861788441317, -17.48830818005195908 ) ) ;
#20815 = LINE ( 'NONE', #4711, #16593 ) ;
#20816 = EDGE_LOOP ( 'NONE', ( #17370, #7475, #10381, #19808, #10006, #10436 ) ) ;
#20817 = AXIS2_PLACEMENT_3D ( 'NONE', #3998, #13756, #10340 ) ;
#20818 = DIRECTION ( 'NONE',  ( -0.5000000000000049960, 0.8660254037844357100, -0.000000000000000000 ) ) ;
#20819 = EDGE_CURVE ( 'NONE', #10374, #10151, #18869, .T. ) ;
#20820 = ORIENTED_EDGE ( 'NONE', *, *, #20131, .T. ) ;
#20821 = CONICAL_SURFACE ( 'NONE', #1547, 3.309499999999999886, 0.7853981633974501664 ) ;
#20822 = CARTESIAN_POINT ( 'NONE',  ( 208.9194833127196489, 31.78152281641241572, -14.00000000000007816 ) ) ;
#20823 = FACE_OUTER_BOUND ( 'NONE', #13005, .T. ) ;
#20824 = VECTOR ( 'NONE', #17279, 1000.000000000000000 ) ;
#20825 = DIRECTION ( 'NONE',  ( 0.5016613886297335290, 0.000000000000000000, 0.8650640734408565624 ) ) ;
#20826 = CARTESIAN_POINT ( 'NONE',  ( 218.5491876009870680, 37.69061213431084667, -11.78314368930802303 ) ) ;
#20827 = VERTEX_POINT ( 'NONE', #2339 ) ;
#20828 = CLOSED_SHELL ( 'NONE', ( #9530, #3168, #4628, #15128, #15548, #1734, #13070, #1398, #8039, #2877, #822, #16909, #13438, #6252, #16904, #393, #20275, #11226, #15216, #5038, #9427, #20365, #6354, #3475, #293, #7591, #14577 ) ) ;
#20829 = DIRECTION ( 'NONE',  ( 0.5000000000000052180, -0.8660254037844355990, 2.220446049250312588E-16 ) ) ;
#20830 = CARTESIAN_POINT ( 'NONE',  ( -3.845968677233049693, 46.83741237530080070, -2.937884555500025474 ) ) ;
#20831 = CARTESIAN_POINT ( 'NONE',  ( 206.5868379288083645, 3.916477399883220745, -1.717498466822807490 ) ) ;
#20832 = AXIS2_PLACEMENT_3D ( 'NONE', #304, #19906, #13562 ) ;
#20833 = CARTESIAN_POINT ( 'NONE',  ( 5.000000000000004441, 2.342598717236899830, -4.057500000000030305 ) ) ;
#20834 = CARTESIAN_POINT ( 'NONE',  ( 218.2125699425740493, 38.47956922221203513, -13.53966000285509530 ) ) ;
#20836 = VERTEX_POINT ( 'NONE', #7398 ) ;
#20835 = VERTEX_POINT ( 'NONE', #18656 ) ;
#20837 = ORIENTED_EDGE ( 'NONE', *, *, #13893, .T. ) ;
#20838 = ORIENTED_EDGE ( 'NONE', *, *, #20521, .F. ) ;
#20839 = DIRECTION ( 'NONE',  ( 0.000000000000000000, 0.000000000000000000, -1.000000000000000000 ) ) ;
#20840 = DIRECTION ( 'NONE',  ( -0.9885408208161367005, 0.000000000000000000, 0.1509537862398905028 ) ) ;
#20841 = CARTESIAN_POINT ( 'NONE',  ( -7.090779867332545727, 80.00000000007909762, -8.779353540718647153 ) ) ;
#20842 =( BOUNDED_CURVE ( )  B_SPLINE_CURVE ( 3, ( #5118, #1642, #154, #11602 ),
 .UNSPECIFIED., .F., .F. ) 
 B_SPLINE_CURVE_WITH_KNOTS ( ( 4, 4 ),
 ( 1.404087049333884217E-16, 1.570796326794897002 ),
 .UNSPECIFIED. ) 
 CURVE ( )  GEOMETRIC_REPRESENTATION_ITEM ( )  RATIONAL_B_SPLINE_CURVE ( ( 1.000000000000000000, 0.8047378541243649375, 0.8047378541243649375, 1.000000000000000000 ) ) 
 REPRESENTATION_ITEM ( '' )  );
#20843 = VERTEX_POINT ( 'NONE', #17274 ) ;
#20844 = ORIENTED_EDGE ( 'NONE', *, *, #9955, .T. ) ;
#20845 = DIRECTION ( 'NONE',  ( 0.8660254037844360431, 0.5000000000000045519, 0.000000000000000000 ) ) ;
#20846 = CARTESIAN_POINT ( 'NONE',  ( 195.0945143319839872, 3.400519391596340757, -15.43274561385865695 ) ) ;
#20847 = CARTESIAN_POINT ( 'NONE',  ( -31.92009862592069069, 62.68228939152199786, 2.325078759242076298 ) ) ;
#20848 = VECTOR ( 'NONE', #10207, 1000.000000000000114 ) ;
#20849 = CARTESIAN_POINT ( 'NONE',  ( 0.000000000000000000, 1.759474945355388398, 3.047499999999996767 ) ) ;
#20850 = VERTEX_POINT ( 'NONE', #10472 ) ;
#20851 = ORIENTED_EDGE ( 'NONE', *, *, #14736, .F. ) ;
#20852 = TOROIDAL_SURFACE ( 'NONE', #8316, 4.400000000000000355, 0.4000000000000000222 ) ;
#20853 = DIRECTION ( 'NONE',  ( 0.5000000000000052180, -0.8660254037844355990, -1.665334536937734318E-16 ) ) ;
#20854 = VECTOR ( 'NONE', #17993, 1000.000000000000114 ) ;
#20855 = DIRECTION ( 'NONE',  ( 0.5000000000000049960, -0.8660254037844358210, 0.000000000000000000 ) ) ;
#20856 = CARTESIAN_POINT ( 'NONE',  ( 210.7957517463719057, 12.99668230119596934, -3.627429155984617459 ) ) ;
#20857 = EDGE_CURVE ( 'NONE', #15613, #10630, #2444, .T. ) ;
#20858 = CARTESIAN_POINT ( 'NONE',  ( 226.1456958721146577, 43.01956746017689426, -13.95414044509031548 ) ) ;
#20859 = CARTESIAN_POINT ( 'NONE',  ( -27.53118063582242669, 59.57781814305143797, 4.826340682015764827 ) ) ;
#20860 = FACE_OUTER_BOUND ( 'NONE', #2512, .T. ) ;
#20861 = ORIENTED_EDGE ( 'NONE', *, *, #2537, .F. ) ;
#20862 = CARTESIAN_POINT ( 'NONE',  ( -31.99612686838726461, 68.02992772322291160, 2.199708061508754753 ) ) ;
#20863 = CARTESIAN_POINT ( 'NONE',  ( 219.5629955745448285, 35.93464521499033282, -17.48830818005195908 ) ) ;
#20864 = CARTESIAN_POINT ( 'NONE',  ( 60.60228022274862525, 122.9901410505958523, 41.00000000000001421 ) ) ;
#20865 = CIRCLE ( 'NONE', #15825, 3.845804376225747667 ) ;
#20866 = EDGE_LOOP ( 'NONE', ( #12048, #11346, #16594, #17458, #5220, #17885, #7160, #19599, #2631, #12187, #11681, #8429 ) ) ;
#20867 = CARTESIAN_POINT ( 'NONE',  ( 79.17481878663886619, 68.98945691342343878, 0.4213564493606052896 ) ) ;
#20868 = ORIENTED_EDGE ( 'NONE', *, *, #10687, .F. ) ;
#20869 = ORIENTED_EDGE ( 'NONE', *, *, #3653, .F. ) ;
#20870 = FACE_OUTER_BOUND ( 'NONE', #17156, .T. ) ;
#20871 = EDGE_CURVE ( 'NONE', #3434, #437, #8897, .T. ) ;
#20872 = CARTESIAN_POINT ( 'NONE',  ( -29.55702837821359097, 79.40496982188669506, -8.308226455662120813 ) ) ;
#20873 = ITEM_DEFINED_TRANSFORMATION ( 'NONE', 'NONE', #19566,  #18233 ) ;
#20874 = CARTESIAN_POINT ( 'NONE',  ( 200.3591165883520659, 22.22039063021986038, -14.00000000000005507 ) ) ;
#20875 = ORIENTED_EDGE ( 'NONE', *, *, #9008, .F. ) ;
#20876 = AXIS2_PLACEMENT_3D ( 'NONE', #1682, #3574, #6428 ) ;
#20877 = CARTESIAN_POINT ( 'NONE',  ( 10.40000000000000568, 6.987792986206746511E-16, 5.400000000000040323 ) ) ;
#20878 = CIRCLE ( 'NONE', #13108, 15.00000000000000000 ) ;
#20879 = CARTESIAN_POINT ( 'NONE',  ( 213.9717500725588479, 7.407338323375970646, -24.35247136794745515 ) ) ;
#20880 = CYLINDRICAL_SURFACE ( 'NONE', #15440, 12.47473710546057646 ) ;
#20881 = DIRECTION ( 'NONE',  ( 0.000000000000000000, -0.8660254037844394848, -0.4999999999999986122 ) ) ;
#20882 = EDGE_CURVE ( 'NONE', #2259, #1594, #10366, .T. ) ;
#20883 = EDGE_CURVE ( 'NONE', #14976, #17359, #849, .T. ) ;
#20884 = FACE_OUTER_BOUND ( 'NONE', #6532, .T. ) ;
#20885 = CARTESIAN_POINT ( 'NONE',  ( 221.6773453713352353, 32.27248394197634696, -14.91677899116122319 ) ) ;
#20886 = CARTESIAN_POINT ( 'NONE',  ( 227.9553588074475670, 39.88513931160575510, -14.00000000000005507 ) ) ;
#20887 = CARTESIAN_POINT ( 'NONE',  ( 208.0983737146324870, 5.661548828456886895, -14.00000000000005507 ) ) ;
#20888 = FACE_OUTER_BOUND ( 'NONE', #11608, .T. ) ;
#20889 = ORIENTED_EDGE ( 'NONE', *, *, #11234, .T. ) ;
#20890 = LINE ( 'NONE', #20585, #10139 ) ;
#20891 = CARTESIAN_POINT ( 'NONE',  ( 82.14226734681926700, 57.73183364759933767, -0.9146047477486081156 ) ) ;
#20892 = EDGE_CURVE ( 'NONE', #18441, #18887, #20571, .T. ) ;
#20893 = AXIS2_PLACEMENT_3D ( 'NONE', #2730, #7485, #13978 ) ;
#20894 = DIRECTION ( 'NONE',  ( 1.000000000000000000, 0.000000000000000000, 0.000000000000000000 ) ) ;
#20895 = CARTESIAN_POINT ( 'NONE',  ( -20.90976142674579563, 14.76829926076707089, 0.9456440915044569406 ) ) ;
#20896 = VECTOR ( 'NONE', #14647, 1000.000000000000114 ) ;
#20898 = VERTEX_POINT ( 'NONE', #1171 ) ;
#20897 = ORIENTED_EDGE ( 'NONE', *, *, #13268, .T. ) ;
#20899 = ORIENTED_EDGE ( 'NONE', *, *, #8161, .F. ) ;
#20900 = ORIENTED_EDGE ( 'NONE', *, *, #20892, .F. ) ;
#20901 = EDGE_CURVE ( 'NONE', #14150, #2303, #17074, .T. ) ;
#20902 = CYLINDRICAL_SURFACE ( 'NONE', #13771, 5.000000000000002665 ) ;
#20903 = ORIENTED_EDGE ( 'NONE', *, *, #7976, .F. ) ;
#20904 = CARTESIAN_POINT ( 'NONE',  ( 213.2794616557154939, 7.007645419554564548, -26.10173121575784450 ) ) ;
#20905 = CARTESIAN_POINT ( 'NONE',  ( -32.89400105397312046, 77.84073441274443894, -4.744404894156348362 ) ) ;
#20906 = CARTESIAN_POINT ( 'NONE',  ( 190.1957632562343008, 15.84194504888569988, -7.132002368301173512 ) ) ;
#20907 = ORIENTED_EDGE ( 'NONE', *, *, #9132, .F. ) ;
#20908 = EDGE_CURVE ( 'NONE', #12371, #12475, #16187, .T. ) ;
#20909 = CARTESIAN_POINT ( 'NONE',  ( 189.6713070174558311, 31.72030020615783386, -19.00000000000004263 ) ) ;
#20910 = AXIS2_PLACEMENT_3D ( 'NONE', #7232, #3953, #17205 ) ;
#20911 = DIRECTION ( 'NONE',  ( 0.8660254037844380415, 0.5000000000000014433, 0.000000000000000000 ) ) ;
#20912 = CARTESIAN_POINT ( 'NONE',  ( 218.3021006999761937, 38.11857920074643857, -12.62147488791602790 ) ) ;
#20913 = ORIENTED_EDGE ( 'NONE', *, *, #1267, .F. ) ;
#20914 = CARTESIAN_POINT ( 'NONE',  ( 218.8798129321970976, 10.24100973658777924, -16.73990883341947367 ) ) ;
#20915 = CARTESIAN_POINT ( 'NONE',  ( 209.7298162261493815, 27.11993578943074823, -11.13829696442610029 ) ) ;
#20916 = EDGE_CURVE ( 'NONE', #5375, #14580, #13890, .T. ) ;
#20917 = ORIENTED_EDGE ( 'NONE', *, *, #10676, .F. ) ;
#20918 = CARTESIAN_POINT ( 'NONE',  ( 228.5829838626408446, 38.79806082790808830, -10.60500809762013752 ) ) ;
#20919 = VERTEX_POINT ( 'NONE', #9096 ) ;
#20920 = CIRCLE ( 'NONE', #2671, 3.902363844300875240 ) ;
#20921 = CARTESIAN_POINT ( 'NONE',  ( 210.0696016554955463, 29.36982461651845711, -11.49990028153587218 ) ) ;
#20922 = CYLINDRICAL_SURFACE ( 'NONE', #8840, 5.999999999999989342 ) ;
#20923 = DIRECTION ( 'NONE',  ( 0.8660254037844360431, 0.5000000000000044409, -5.976026924694053325E-17 ) ) ;
#20924 = EDGE_CURVE ( 'NONE', #14504, #18516, #15595, .T. ) ;
#20925 =( GEOMETRIC_REPRESENTATION_CONTEXT ( 3 ) GLOBAL_UNCERTAINTY_ASSIGNED_CONTEXT ( ( #243 ) ) GLOBAL_UNIT_ASSIGNED_CONTEXT ( ( #16702, #11934, #3645 ) ) REPRESENTATION_CONTEXT ( 'NONE', 'WORKASPACE' ) );
#20926 = DIRECTION ( 'NONE',  ( 0.000000000000000000, -0.7500000000000006661, -0.6614378277661467909 ) ) ;
#20927 = CARTESIAN_POINT ( 'NONE',  ( -26.97244842139108911, 6.114691179184633008, -6.023624517011918478 ) ) ;
#20928 = B_SPLINE_CURVE_WITH_KNOTS ( 'NONE', 3,
 ( #9557, #7547, #16054, #14041 ),
 .UNSPECIFIED., .F., .F.,
 ( 4, 4 ),
 ( 3.079010676197774585E-05, 0.0008847758447462670487 ),
 .UNSPECIFIED. ) ;
#20929 = VERTEX_POINT ( 'NONE', #2863 ) ;
#20930 = CARTESIAN_POINT ( 'NONE',  ( 79.17199999999999704, 5.776289300541406836E-16, -4.999999999999999112 ) ) ;
#20931 = EDGE_CURVE ( 'NONE', #11210, #15101, #3065, .T. ) ;
#20932 = AXIS2_PLACEMENT_3D ( 'NONE', #15932, #3096, #1606 ) ;
#20933 = VERTEX_POINT ( 'NONE', #12617 ) ;
#20934 = DIRECTION ( 'NONE',  ( -1.000000000000000000, 0.000000000000000000, 0.000000000000000000 ) ) ;
#20935 = CARTESIAN_POINT ( 'NONE',  ( -9.881800664016866520, 50.28787322564019036, -15.42703672695025752 ) ) ;
#20936 = CARTESIAN_POINT ( 'NONE',  ( 221.7398910005669563, 32.78200010370005657, -11.55788255683066268 ) ) ;
#20937 = EDGE_CURVE ( 'NONE', #8299, #18096, #11615, .T. ) ;
#20938 = PRODUCT_DEFINITION_FORMATION_WITH_SPECIFIED_SOURCE ( 'ANY', '', #5672, .NOT_KNOWN. ) ;
#20939 = CARTESIAN_POINT ( 'NONE',  ( 213.4352746215837726, 14.52061154373172158, -6.376588578941996488 ) ) ;
#20940 = CARTESIAN_POINT ( 'NONE',  ( -25.76165165806668611, 45.05596121145901378, -7.817108404872156413 ) ) ;
#20942 = ORIENTED_EDGE ( 'NONE', *, *, #14048, .F. ) ;
#20941 = ORIENTED_EDGE ( 'NONE', *, *, #8782, .F. ) ;
#20943 = EDGE_LOOP ( 'NONE', ( #8791, #7065, #395, #10023, #7762 ) ) ;
#20944 = ORIENTED_EDGE ( 'NONE', *, *, #4420, .T. ) ;
#20945 = CARTESIAN_POINT ( 'NONE',  ( 199.4613974551745059, 6.452789800082466165, -23.47937149798923429 ) ) ;
#20946 = CARTESIAN_POINT ( 'NONE',  ( 198.2729934012025979, -1.398743842967087314, -15.41218500610144559 ) ) ;
#20947 = CARTESIAN_POINT ( 'NONE',  ( 201.8794782033450588, 11.97286728836375680, -26.96550585544242296 ) ) ;
#20948 = NEXT_ASSEMBLY_USAGE_OCCURRENCE ( 'NAUO1', ' ', ' ', #8107, #19727, $ ) ;
#20949 = NEXT_ASSEMBLY_USAGE_OCCURRENCE ( 'NAUO2', ' ', ' ', #8107, #11582, $ ) ;
#20950 = NEXT_ASSEMBLY_USAGE_OCCURRENCE ( 'NAUO3', ' ', ' ', #8107, #19104, $ ) ;
#20951 = NEXT_ASSEMBLY_USAGE_OCCURRENCE ( 'NAUO4', ' ', ' ', #8107, #7172, $ ) ;
#20952 = NEXT_ASSEMBLY_USAGE_OCCURRENCE ( 'NAUO5', ' ', ' ', #8107, #10936, $ ) ;
#20953 = NEXT_ASSEMBLY_USAGE_OCCURRENCE ( 'NAUO6', ' ', ' ', #8107, #12880, $ ) ;
#20954 = NEXT_ASSEMBLY_USAGE_OCCURRENCE ( 'NAUO7', ' ', ' ', #8107, #13142, $ ) ;
#20955 = NEXT_ASSEMBLY_USAGE_OCCURRENCE ( 'NAUO8', ' ', ' ', #8107, #10936, $ ) ;
#20956 = NEXT_ASSEMBLY_USAGE_OCCURRENCE ( 'NAUO9', ' ', ' ', #8107, #16891, $ ) ;
#20957 = NEXT_ASSEMBLY_USAGE_OCCURRENCE ( 'NAUO10', ' ', ' ', #8107, #15369, $ ) ;
#20958 = NEXT_ASSEMBLY_USAGE_OCCURRENCE ( 'NAUO11', ' ', ' ', #8107, #5599, $ ) ;
#20959 = NEXT_ASSEMBLY_USAGE_OCCURRENCE ( 'NAUO12', ' ', ' ', #8107, #3795, $ ) ;
#20960 = NEXT_ASSEMBLY_USAGE_OCCURRENCE ( 'NAUO13', ' ', ' ', #8107, #8724, $ ) ;
#20961=COLOUR_RGB('Dark Blue',0.08,0.2,0.34);
#20962=FILL_AREA_STYLE_COLOUR('',#20961);
#20963=FILL_AREA_STYLE('',(#20962));
#20964=SURFACE_STYLE_FILL_AREA(#20963);
#20965=SURFACE_SIDE_STYLE('',(#20964));
#20966=SURFACE_STYLE_USAGE(.BOTH.,#20965);
#20967=PRESENTATION_STYLE_ASSIGNMENT((#20966));
#20968=COLOUR_RGB('Light Blue',0.38,0.62,0.78);
#20969=FILL_AREA_STYLE_COLOUR('',#20968);
#20970=FILL_AREA_STYLE('',(#20969));
#20971=SURFACE_STYLE_FILL_AREA(#20970);
#20972=SURFACE_SIDE_STYLE('',(#20971));
#20973=SURFACE_STYLE_USAGE(.BOTH.,#20972);
#20974=PRESENTATION_STYLE_ASSIGNMENT((#20973));
#20975=COLOUR_RGB('Sky Blue',0.24,0.69,0.87);
#20976=FILL_AREA_STYLE_COLOUR('',#20975);
#20977=FILL_AREA_STYLE('',(#20976));
#20978=SURFACE_STYLE_FILL_AREA(#20977);
#20979=SURFACE_SIDE_STYLE('',(#20978));
#20980=SURFACE_STYLE_USAGE(.BOTH.,#20979);
#20981=PRESENTATION_STYLE_ASSIGNMENT((#20980));
#20982=COLOUR_RGB('Grey',0.48,0.52,0.57);
#20983=FILL_AREA_STYLE_COLOUR('',#20982);
#20984=FILL_AREA_STYLE('',(#20983));
#20985=SURFACE_STYLE_FILL_AREA(#20984);
#20986=SURFACE_SIDE_STYLE('',(#20985));
#20987=SURFACE_STYLE_USAGE(.BOTH.,#20986);
#20988=PRESENTATION_STYLE_ASSIGNMENT((#20987));
#20989=COLOUR_RGB('Black',0.12,0.14,0.17);
#20990=FILL_AREA_STYLE_COLOUR('',#20989);
#20991=FILL_AREA_STYLE('',(#20990));
#20992=SURFACE_STYLE_FILL_AREA(#20991);
#20993=SURFACE_SIDE_STYLE('',(#20992));
#20994=SURFACE_STYLE_USAGE(.BOTH.,#20993);
#20995=PRESENTATION_STYLE_ASSIGNMENT((#20994));
#20996=COLOUR_RGB('Off White',0.89,0.88,0.83);
#20997=FILL_AREA_STYLE_COLOUR('',#20996);
#20998=FILL_AREA_STYLE('',(#20997));
#20999=SURFACE_STYLE_FILL_AREA(#20998);
#21000=SURFACE_SIDE_STYLE('',(#20999));
#21001=SURFACE_STYLE_USAGE(.BOTH.,#21000);
#21002=PRESENTATION_STYLE_ASSIGNMENT((#21001));
ENDSEC;
END-ISO-10303-21;
